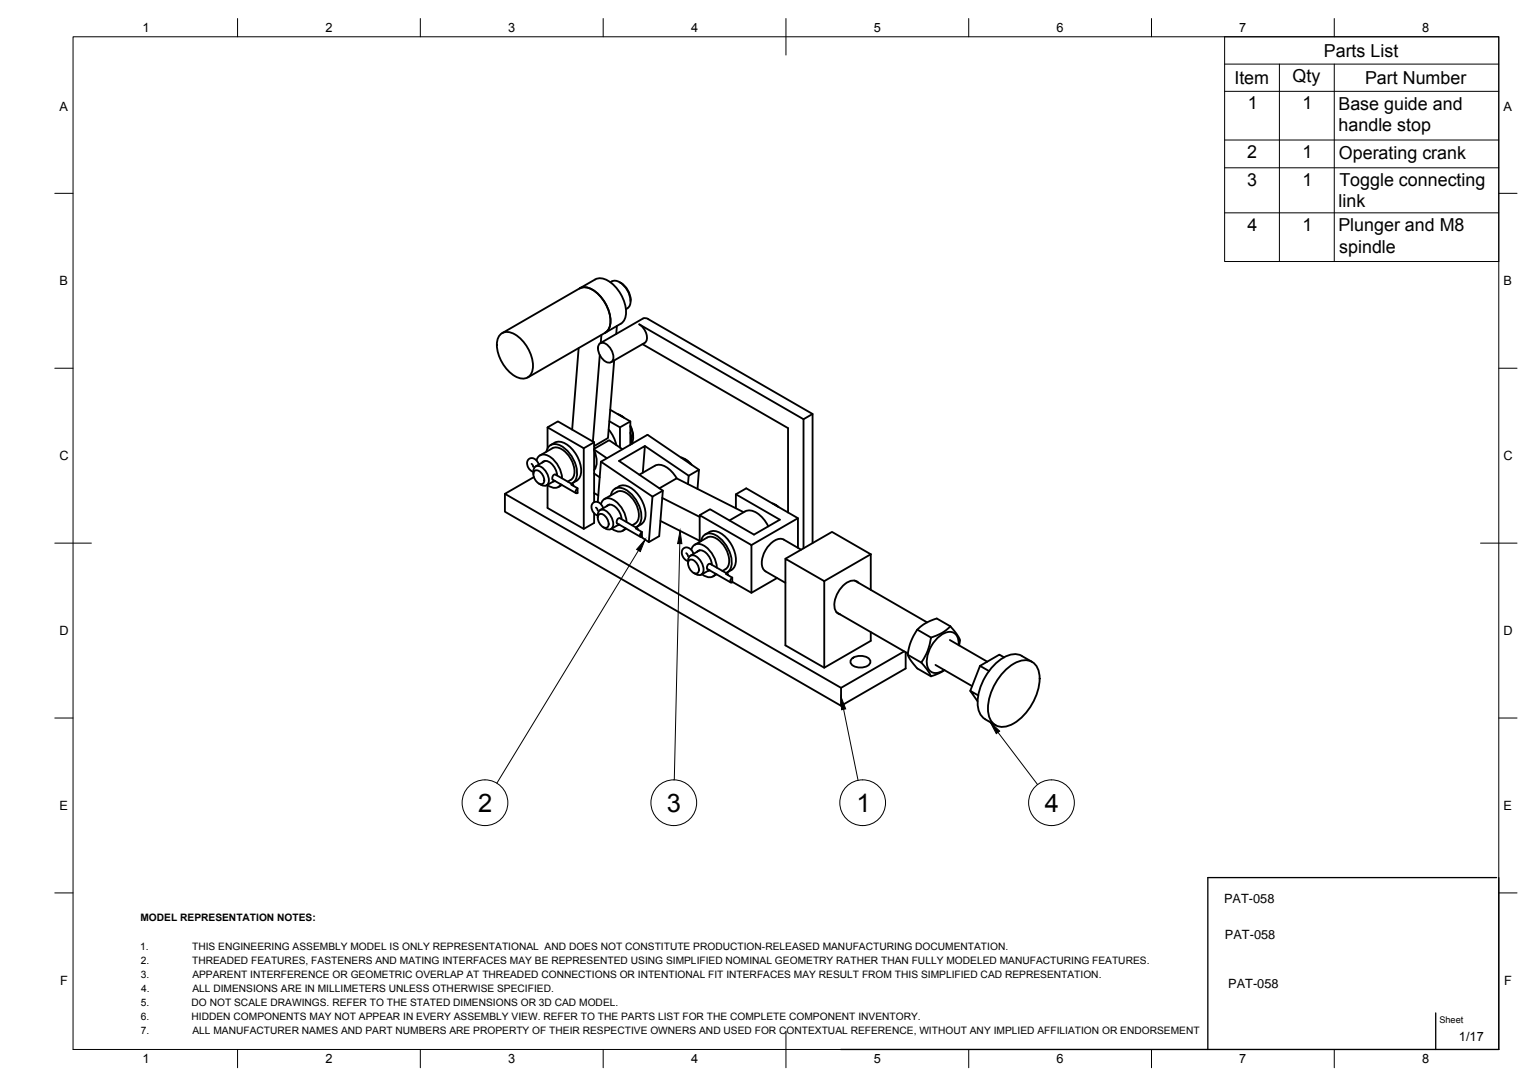
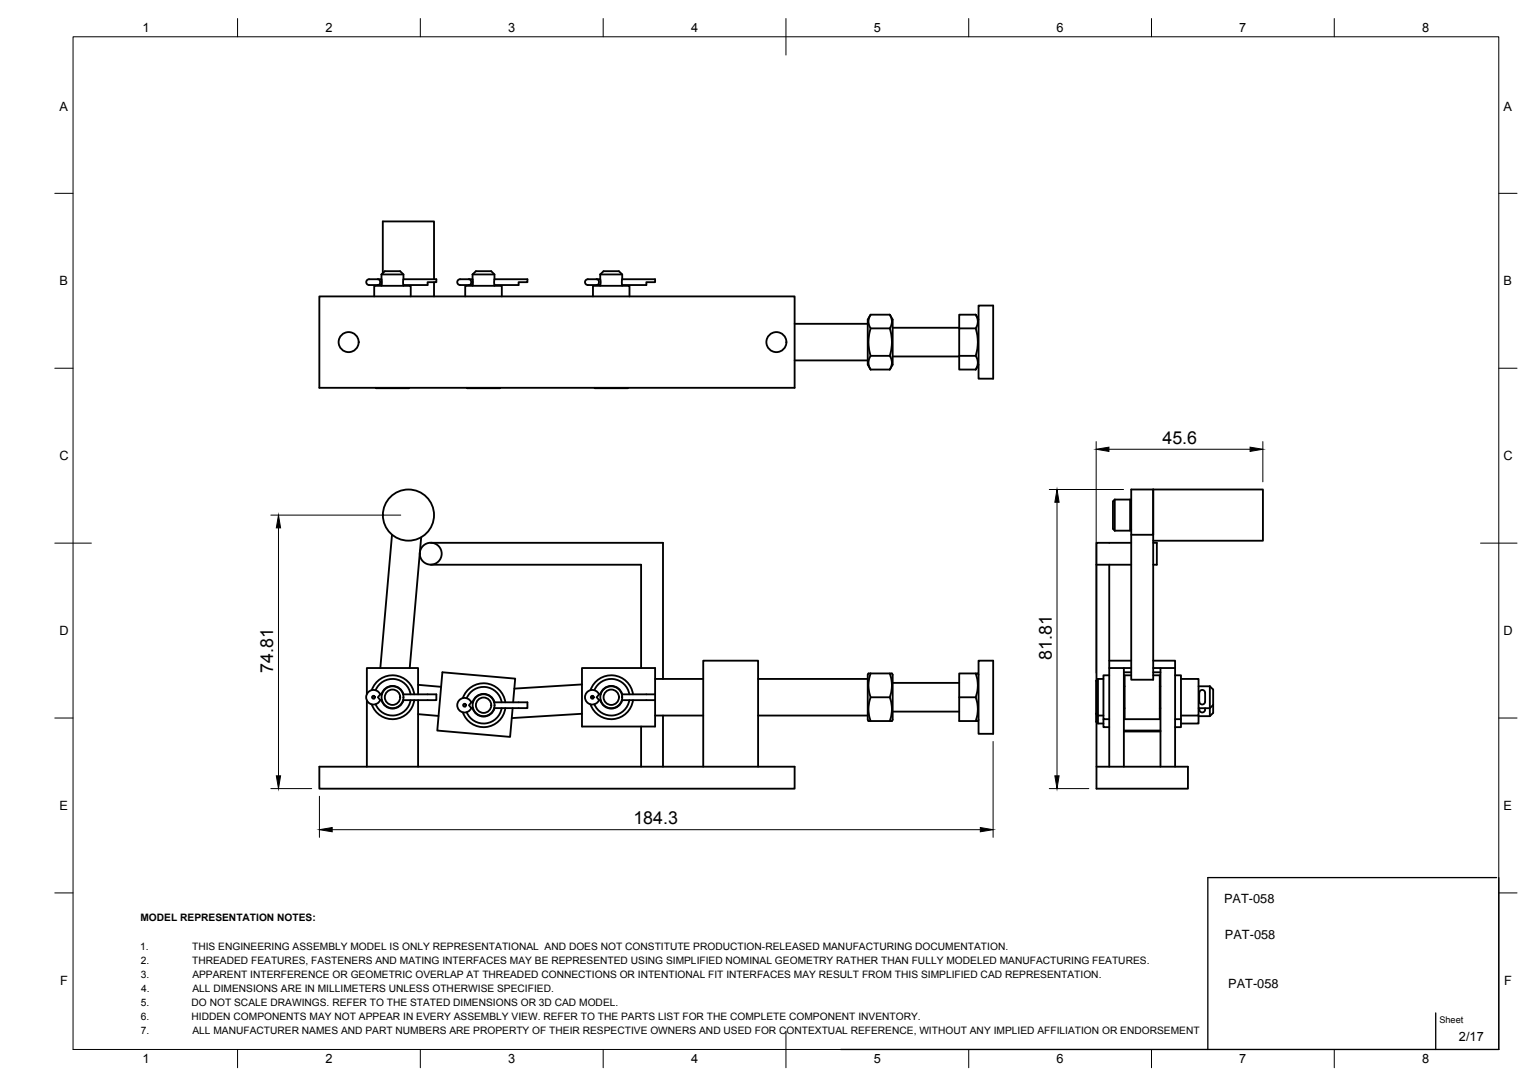
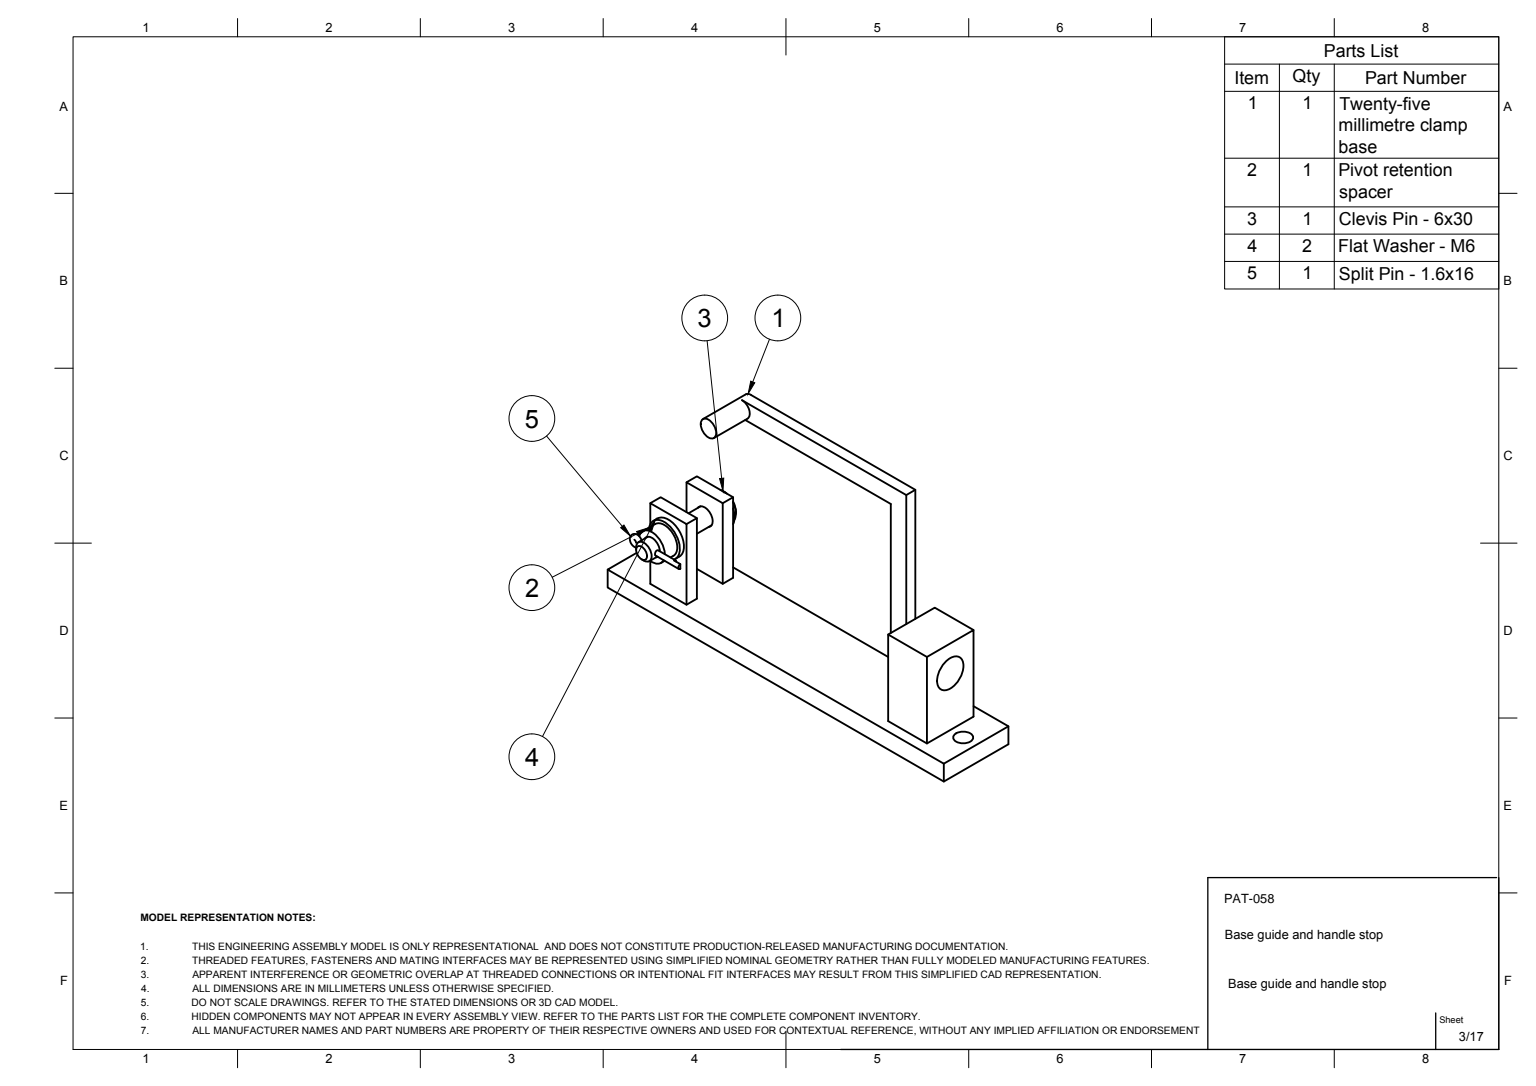
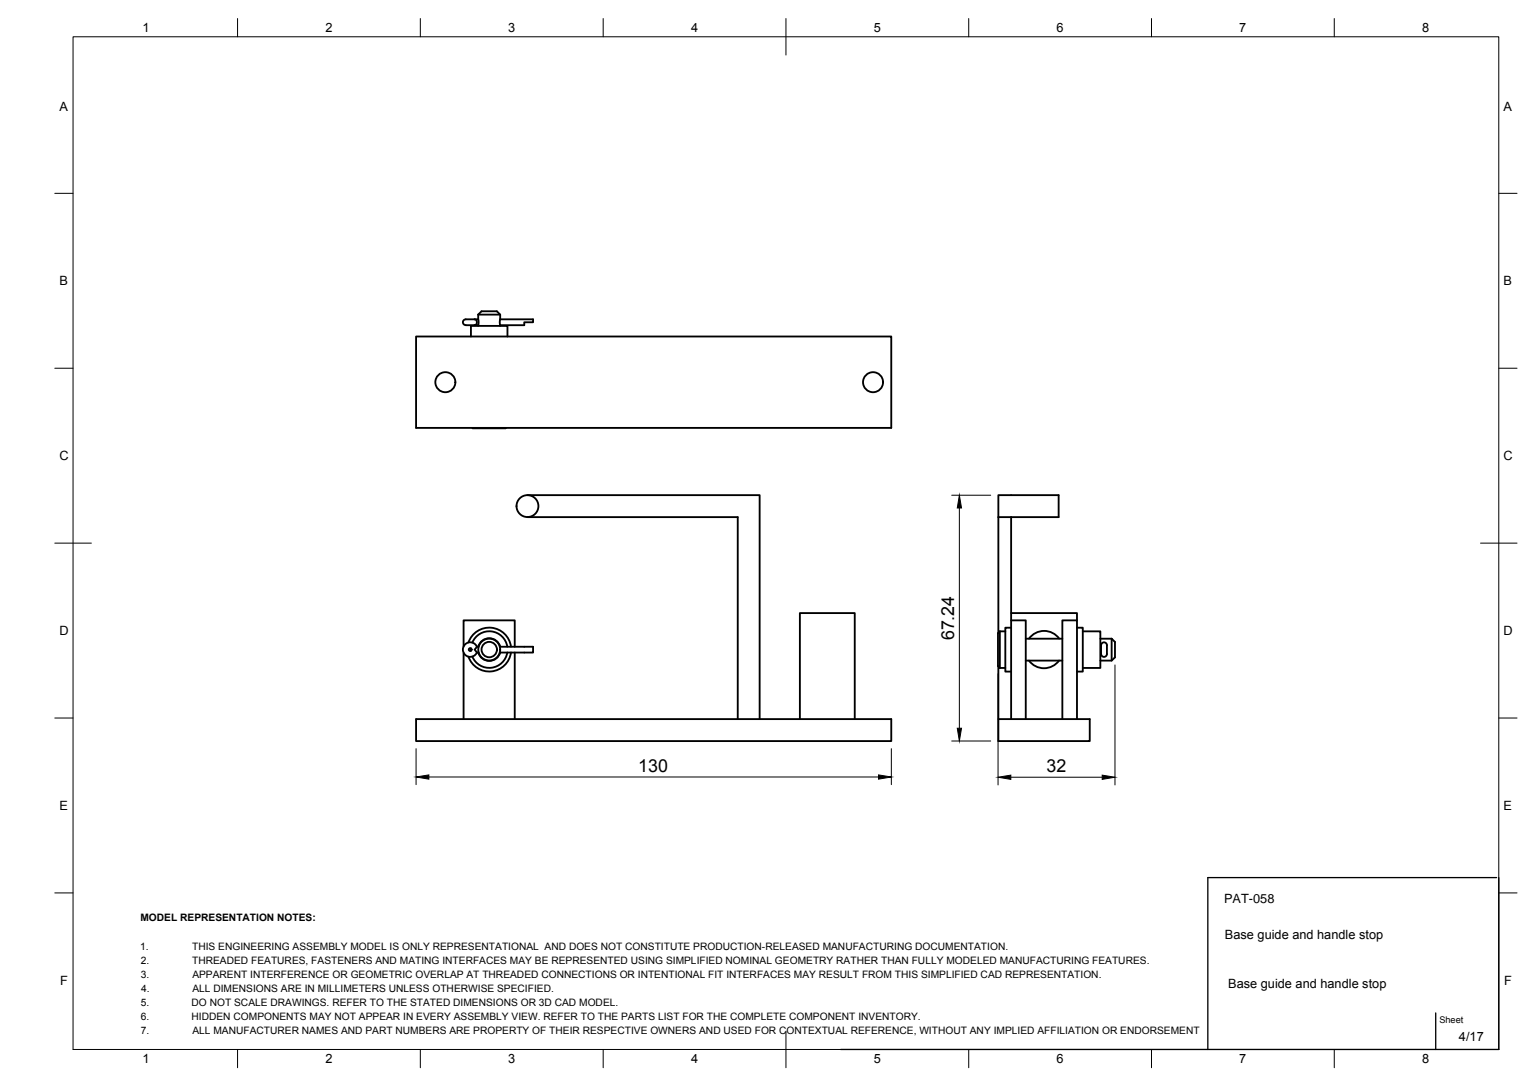
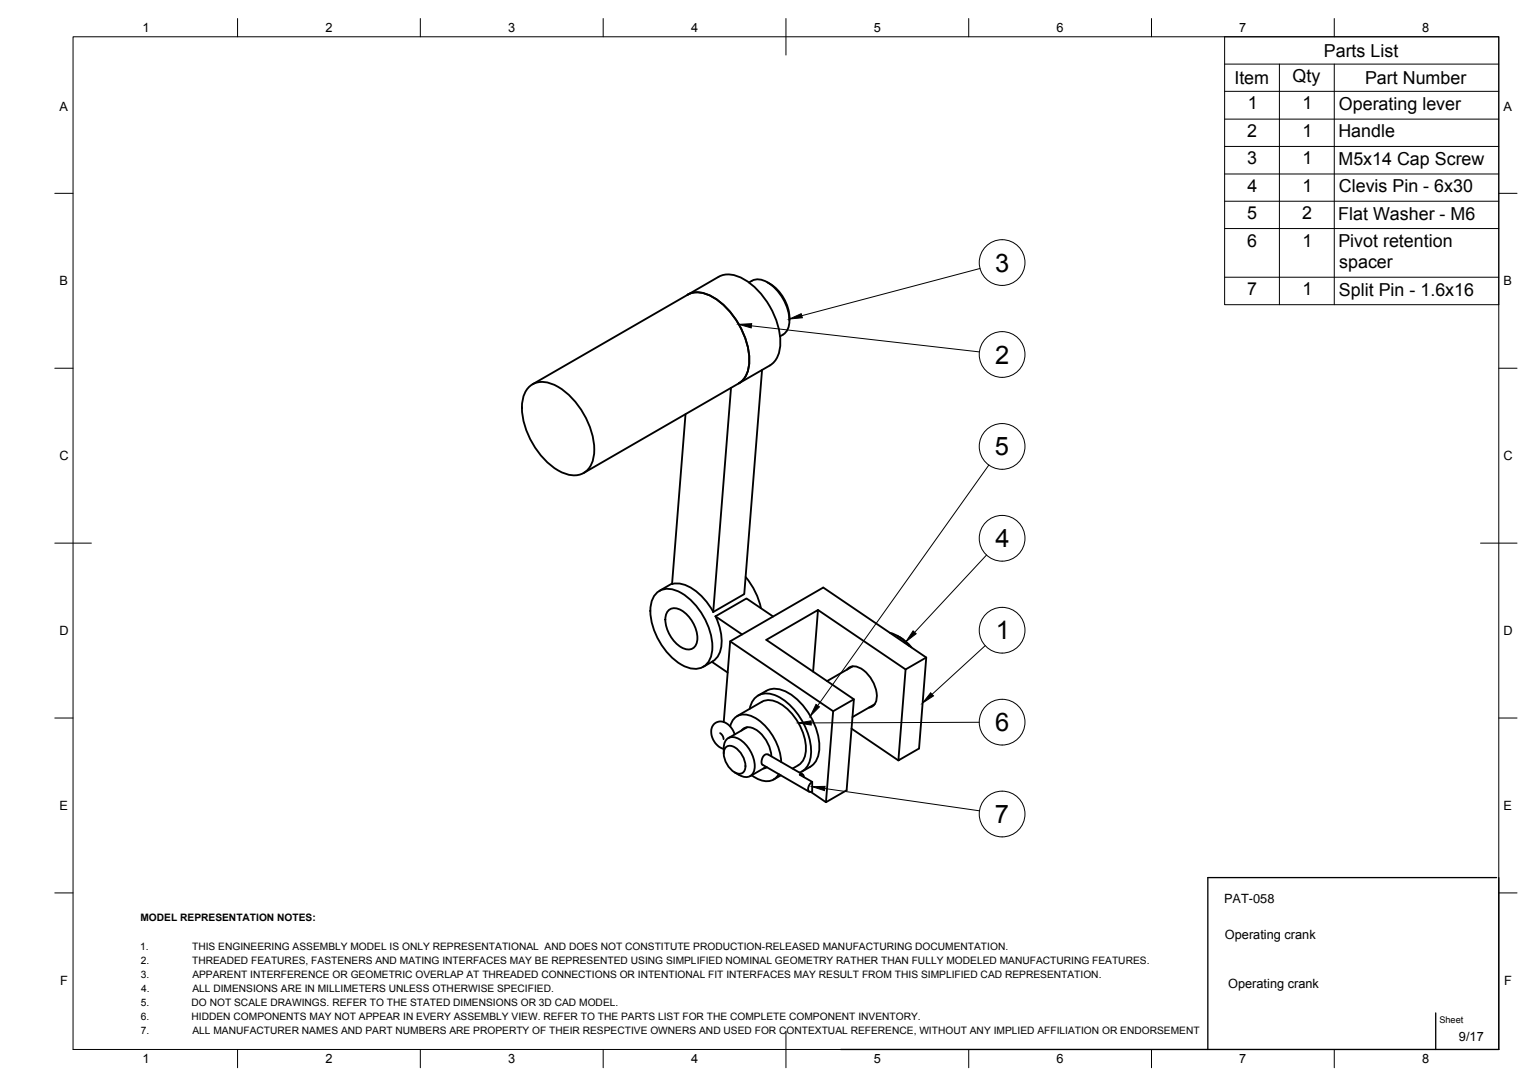
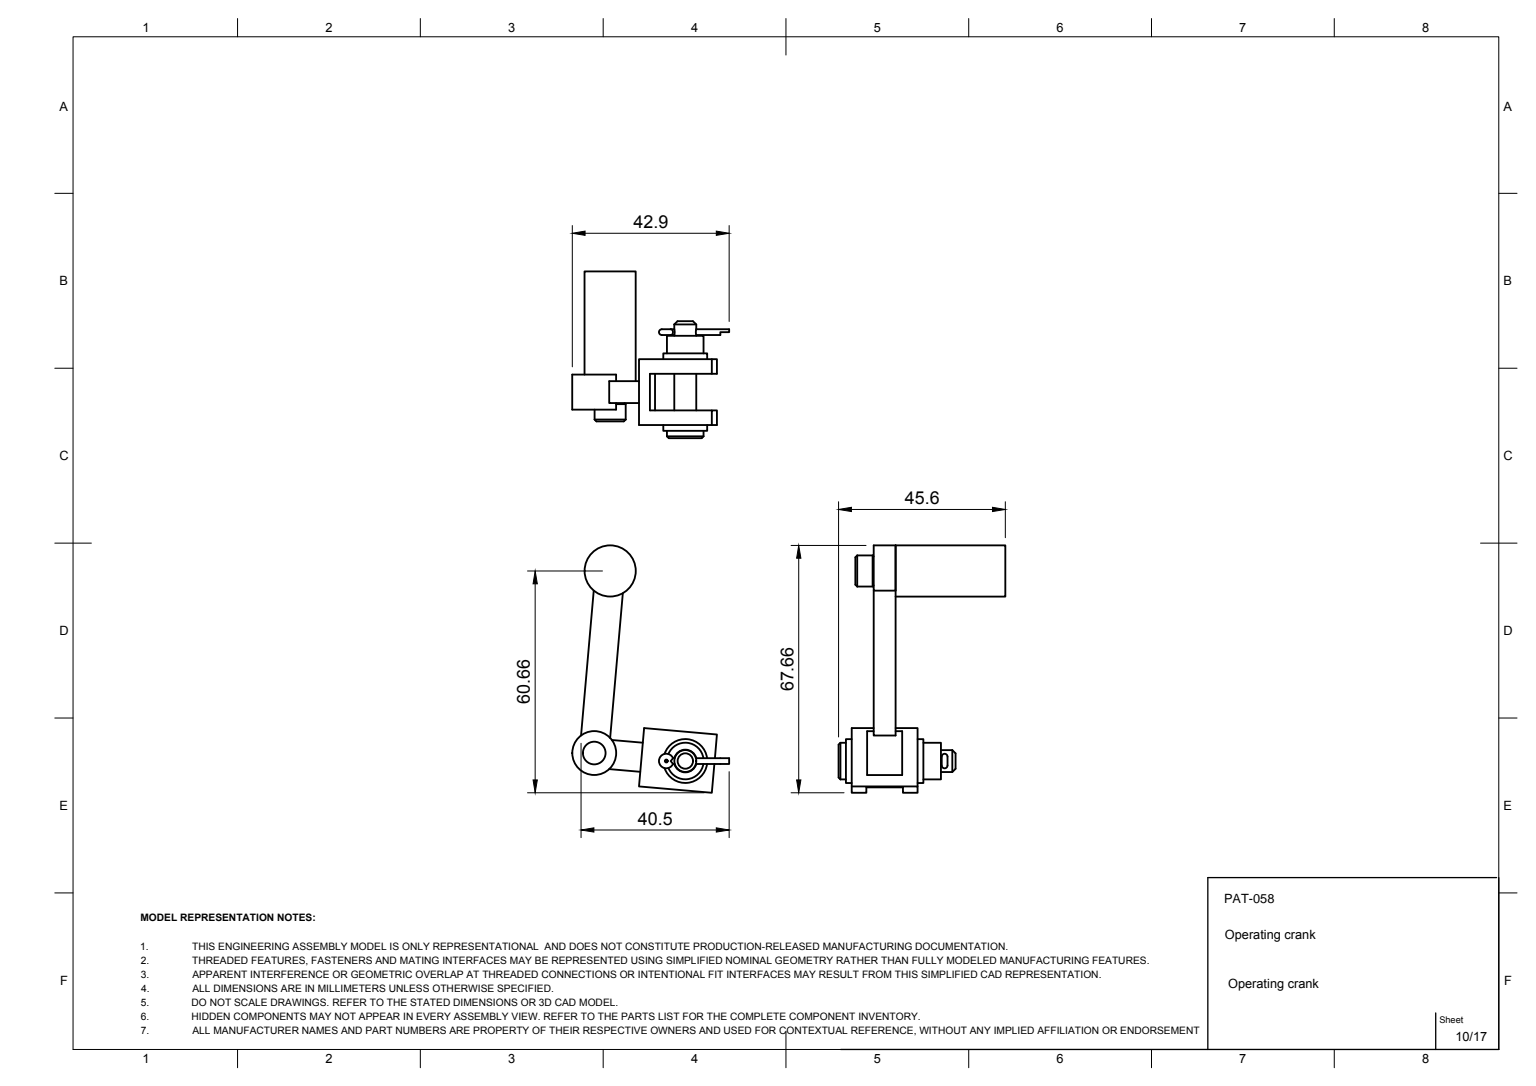
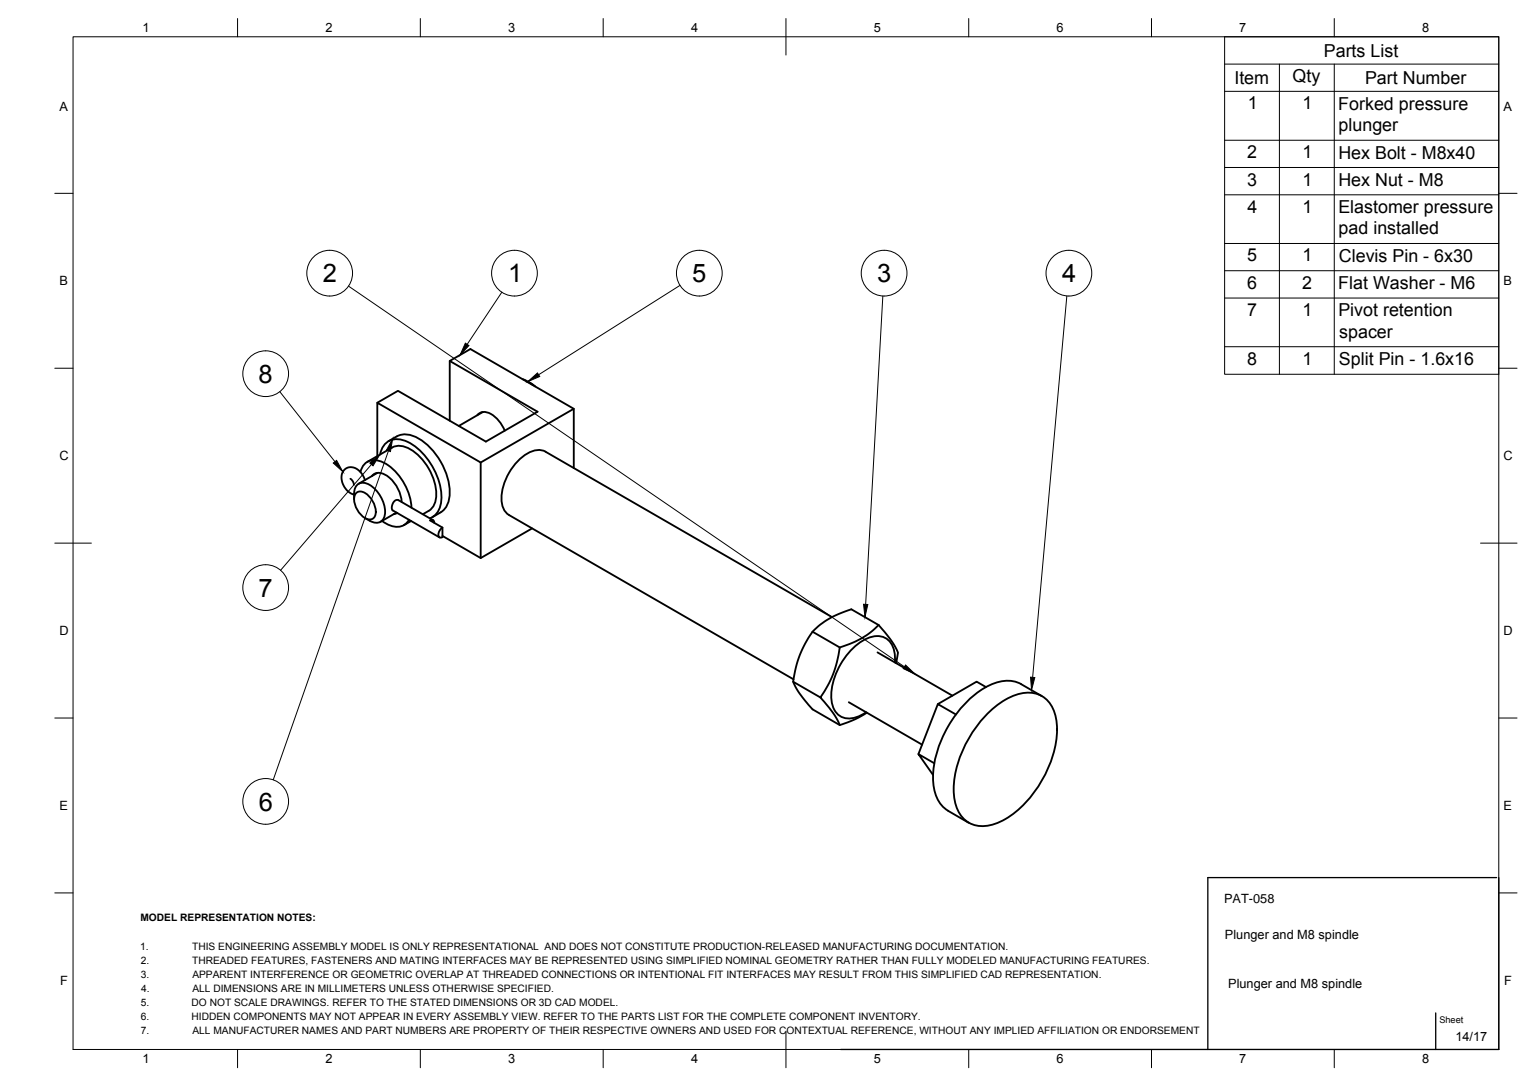
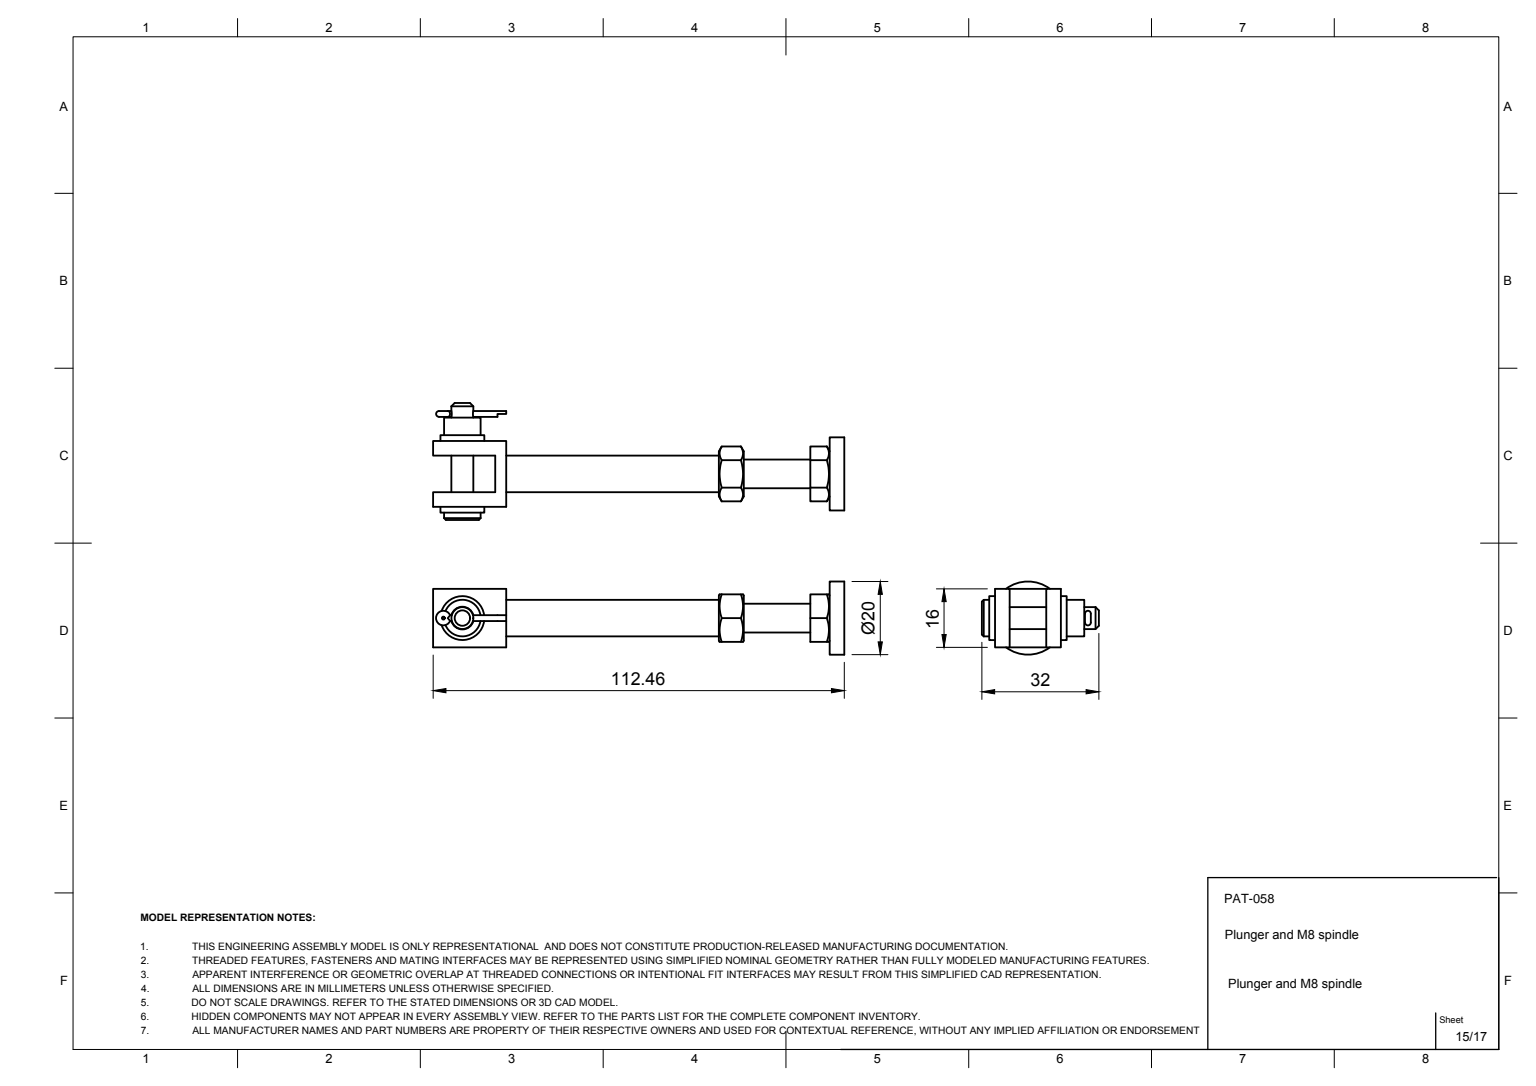
ISO-10303-21;
HEADER;
/* Generated by software containing ST-Developer
 * from STEP Tools, Inc. (www.steptools.com) 
 */

FILE_DESCRIPTION(
/* description */ ('Horizontal push-pull toggle clamp'),
/* implementation_level */ '2;1');

FILE_NAME(
/* name */ 'PAT-058',
/* time_stamp */ '2026-10-27T21:21:09-07:00',
/* author */ (''),
/* organization */ (''),
/* preprocessor_version */ 'ST-DEVELOPER v20.2',
/* originating_system */ 'Autodesk Translation Framework v15.17.0.0',
/* authorisation */ '');

FILE_SCHEMA (('AUTOMOTIVE_DESIGN { 1 0 10303 214 3 1 1 }'));
ENDSEC;

DATA;
#10=MECHANICAL_DESIGN_GEOMETRIC_PRESENTATION_REPRESENTATION('',(#185,#186,
#187,#188,#189,#190,#191,#192,#193,#194,#195,#196,#197),#4791);
#11=TOROIDAL_SURFACE('',#3033,0.12,0.08);
#12=B_SPLINE_CURVE_WITH_KNOTS('',3,(#4522,#4523,#4524,#4525,#4526,#4527,
#4528,#4529,#4530,#4531),.UNSPECIFIED.,.F.,.F.,(4,2,2,2,4),(0.,0.0302963256060356,
0.0605926512120712,0.090883446720838,0.121174242229605),.UNSPECIFIED.);
#13=B_SPLINE_CURVE_WITH_KNOTS('',3,(#4534,#4535,#4536,#4537,#4538,#4539,
#4540,#4541,#4542,#4543,#4544,#4545,#4546,#4547,#4548,#4549,#4550,#4551,
#4552,#4553,#4554,#4555,#4556,#4557,#4558,#4559,#4560,#4561,#4562,#4563,
#4564,#4565,#4566,#4567),.UNSPECIFIED.,.T.,.F.,(4,2,2,2,2,2,2,2,2,2,2,2,
2,2,2,2,4),(0.,0.0302963256060358,0.0605926512120716,0.0908834467208383,
0.121174242229605,0.151465037738372,0.181755833247138,0.212052158853174,
0.24234848445921,0.272644810065246,0.302941135671282,0.333231931180048,
0.363522726688815,0.393813522197582,0.424104317706349,0.454400643312384,
0.48469696891842),.UNSPECIFIED.);
#14=B_SPLINE_CURVE_WITH_KNOTS('',3,(#4569,#4570,#4571,#4572,#4573,#4574,
#4575,#4576,#4577,#4578),.UNSPECIFIED.,.F.,.F.,(4,2,2,2,4),(0.363522726688815,
0.393813522197581,0.424104317706348,0.454400643312384,0.48469696891842),
 .UNSPECIFIED.);
#15=B_SPLINE_CURVE_WITH_KNOTS('',3,(#4579,#4580,#4581,#4582,#4583,#4584,
#4585,#4586,#4587,#4588,#4589,#4590,#4591,#4592,#4593,#4594,#4595,#4596),
 .UNSPECIFIED.,.F.,.F.,(4,2,2,2,2,2,2,2,4),(0.121174242229605,0.151465037738371,
0.181755833247138,0.212052158853174,0.24234848445921,0.272644810065246,
0.302941135671281,0.333231931180048,0.363522726688815),.UNSPECIFIED.);
#16=B_SPLINE_CURVE_WITH_KNOTS('',3,(#4658,#4659,#4660,#4661,#4662,#4663,
#4664,#4665,#4666,#4667,#4668,#4669,#4670,#4671,#4672,#4673,#4674,#4675,
#4676,#4677,#4678,#4679,#4680,#4681,#4682,#4683),.UNSPECIFIED.,.F.,.F.,
(4,2,2,2,2,2,2,2,2,2,2,2,4),(-0.00054581412719389,0.,0.0281583564005144,
0.0618496465371181,0.0905865724114538,0.120694112793616,0.144966158459363,
0.16923820412511,0.199345744507272,0.228082670381608,0.261773960518212,
0.289932316918681,0.290478131045882),.UNSPECIFIED.);
#17=B_SPLINE_CURVE_WITH_KNOTS('',3,(#4684,#4685,#4686,#4687,#4688,#4689,
#4690,#4691,#4692,#4693,#4694,#4695,#4696,#4697,#4698,#4699,#4700,#4701,
#4702,#4703,#4704,#4705,#4706,#4707,#4708,#4709),.UNSPECIFIED.,.F.,.F.,
(4,2,2,2,2,2,2,2,2,2,2,2,4),(-0.000545814127196571,0.,0.0281583564006391,
0.0618496465374156,0.0905865724118984,0.120694112794215,0.144966158460086,
0.169238204125958,0.199345744508275,0.228082670382758,0.261773960519534,
0.289932316920171,0.29047813104737),.UNSPECIFIED.);
#18=(
BOUNDED_CURVE()
B_SPLINE_CURVE(2,(#4384,#4385,#4386),.UNSPECIFIED.,.F.,.F.)
B_SPLINE_CURVE_WITH_KNOTS((3,3),(0.14973948338295,0.97160236658079),
 .UNSPECIFIED.)
CURVE()
GEOMETRIC_REPRESENTATION_ITEM()
RATIONAL_B_SPLINE_CURVE((1.07140024848292,1.23714644374248,1.07140024848292))
REPRESENTATION_ITEM('')
);
#19=(
BOUNDED_CURVE()
B_SPLINE_CURVE(2,(#4388,#4389,#4390),.UNSPECIFIED.,.F.,.F.)
B_SPLINE_CURVE_WITH_KNOTS((3,3),(0.14973948338295,0.97160236658079),
 .UNSPECIFIED.)
CURVE()
GEOMETRIC_REPRESENTATION_ITEM()
RATIONAL_B_SPLINE_CURVE((1.07140024848292,1.23714644374248,1.07140024848292))
REPRESENTATION_ITEM('')
);
#20=(
BOUNDED_CURVE()
B_SPLINE_CURVE(2,(#4392,#4393,#4394),.UNSPECIFIED.,.F.,.F.)
B_SPLINE_CURVE_WITH_KNOTS((3,3),(0.14973948338295,0.97160236658079),
 .UNSPECIFIED.)
CURVE()
GEOMETRIC_REPRESENTATION_ITEM()
RATIONAL_B_SPLINE_CURVE((1.07140024848292,1.23714644374248,1.07140024848292))
REPRESENTATION_ITEM('')
);
#21=(
BOUNDED_CURVE()
B_SPLINE_CURVE(2,(#4396,#4397,#4398),.UNSPECIFIED.,.F.,.F.)
B_SPLINE_CURVE_WITH_KNOTS((3,3),(0.149739483382949,0.971602366580789),
 .UNSPECIFIED.)
CURVE()
GEOMETRIC_REPRESENTATION_ITEM()
RATIONAL_B_SPLINE_CURVE((1.07140024848292,1.23714644374248,1.07140024848292))
REPRESENTATION_ITEM('')
);
#22=(
BOUNDED_CURVE()
B_SPLINE_CURVE(2,(#4400,#4401,#4402),.UNSPECIFIED.,.F.,.F.)
B_SPLINE_CURVE_WITH_KNOTS((3,3),(0.14973948338295,0.971602366580789),
 .UNSPECIFIED.)
CURVE()
GEOMETRIC_REPRESENTATION_ITEM()
RATIONAL_B_SPLINE_CURVE((1.07140024848292,1.23714644374248,1.07140024848292))
REPRESENTATION_ITEM('')
);
#23=(
BOUNDED_CURVE()
B_SPLINE_CURVE(2,(#4403,#4404,#4405),.UNSPECIFIED.,.F.,.F.)
B_SPLINE_CURVE_WITH_KNOTS((3,3),(0.14973948338295,0.97160236658079),
 .UNSPECIFIED.)
CURVE()
GEOMETRIC_REPRESENTATION_ITEM()
RATIONAL_B_SPLINE_CURVE((1.07140024848292,1.23714644374248,1.07140024848292))
REPRESENTATION_ITEM('')
);
#24=(
BOUNDED_CURVE()
B_SPLINE_CURVE(2,(#4436,#4437,#4438),.UNSPECIFIED.,.F.,.F.)
B_SPLINE_CURVE_WITH_KNOTS((3,3),(0.14973948338295,0.97160236658079),
 .UNSPECIFIED.)
CURVE()
GEOMETRIC_REPRESENTATION_ITEM()
RATIONAL_B_SPLINE_CURVE((1.07140024848292,1.23714644374248,1.07140024848292))
REPRESENTATION_ITEM('')
);
#25=(
BOUNDED_CURVE()
B_SPLINE_CURVE(2,(#4440,#4441,#4442),.UNSPECIFIED.,.F.,.F.)
B_SPLINE_CURVE_WITH_KNOTS((3,3),(0.14973948338295,0.971602366580789),
 .UNSPECIFIED.)
CURVE()
GEOMETRIC_REPRESENTATION_ITEM()
RATIONAL_B_SPLINE_CURVE((1.07140024848292,1.23714644374248,1.07140024848292))
REPRESENTATION_ITEM('')
);
#26=(
BOUNDED_CURVE()
B_SPLINE_CURVE(2,(#4447,#4448,#4449),.UNSPECIFIED.,.F.,.F.)
B_SPLINE_CURVE_WITH_KNOTS((3,3),(0.14973948338295,0.97160236658079),
 .UNSPECIFIED.)
CURVE()
GEOMETRIC_REPRESENTATION_ITEM()
RATIONAL_B_SPLINE_CURVE((1.07140024848292,1.23714644374248,1.07140024848292))
REPRESENTATION_ITEM('')
);
#27=(
BOUNDED_CURVE()
B_SPLINE_CURVE(2,(#4451,#4452,#4453),.UNSPECIFIED.,.F.,.F.)
B_SPLINE_CURVE_WITH_KNOTS((3,3),(0.14973948338295,0.97160236658079),
 .UNSPECIFIED.)
CURVE()
GEOMETRIC_REPRESENTATION_ITEM()
RATIONAL_B_SPLINE_CURVE((1.07140024848292,1.23714644374248,1.07140024848292))
REPRESENTATION_ITEM('')
);
#28=(
BOUNDED_CURVE()
B_SPLINE_CURVE(2,(#4455,#4456,#4457),.UNSPECIFIED.,.F.,.F.)
B_SPLINE_CURVE_WITH_KNOTS((3,3),(0.14973948338295,0.971602366580789),
 .UNSPECIFIED.)
CURVE()
GEOMETRIC_REPRESENTATION_ITEM()
RATIONAL_B_SPLINE_CURVE((1.07140024848292,1.23714644374248,1.07140024848292))
REPRESENTATION_ITEM('')
);
#29=(
BOUNDED_CURVE()
B_SPLINE_CURVE(2,(#4458,#4459,#4460),.UNSPECIFIED.,.F.,.F.)
B_SPLINE_CURVE_WITH_KNOTS((3,3),(0.14973948338295,0.97160236658079),
 .UNSPECIFIED.)
CURVE()
GEOMETRIC_REPRESENTATION_ITEM()
RATIONAL_B_SPLINE_CURVE((1.07140024848292,1.23714644374248,1.07140024848292))
REPRESENTATION_ITEM('')
);
#30=(
BOUNDED_CURVE()
B_SPLINE_CURVE(2,(#4467,#4468,#4469),.UNSPECIFIED.,.F.,.F.)
B_SPLINE_CURVE_WITH_KNOTS((3,3),(0.14973948338295,0.97160236658079),
 .UNSPECIFIED.)
CURVE()
GEOMETRIC_REPRESENTATION_ITEM()
RATIONAL_B_SPLINE_CURVE((1.07140024848292,1.23714644374248,1.07140024848292))
REPRESENTATION_ITEM('')
);
#31=(
BOUNDED_CURVE()
B_SPLINE_CURVE(2,(#4471,#4472,#4473),.UNSPECIFIED.,.F.,.F.)
B_SPLINE_CURVE_WITH_KNOTS((3,3),(0.14973948338295,0.97160236658079),
 .UNSPECIFIED.)
CURVE()
GEOMETRIC_REPRESENTATION_ITEM()
RATIONAL_B_SPLINE_CURVE((1.07140024848292,1.23714644374248,1.07140024848292))
REPRESENTATION_ITEM('')
);
#32=(
BOUNDED_CURVE()
B_SPLINE_CURVE(2,(#4475,#4476,#4477),.UNSPECIFIED.,.F.,.F.)
B_SPLINE_CURVE_WITH_KNOTS((3,3),(0.14973948338295,0.971602366580789),
 .UNSPECIFIED.)
CURVE()
GEOMETRIC_REPRESENTATION_ITEM()
RATIONAL_B_SPLINE_CURVE((1.07140024848292,1.23714644374248,1.07140024848292))
REPRESENTATION_ITEM('')
);
#33=(
BOUNDED_CURVE()
B_SPLINE_CURVE(2,(#4479,#4480,#4481),.UNSPECIFIED.,.F.,.F.)
B_SPLINE_CURVE_WITH_KNOTS((3,3),(0.14973948338295,0.97160236658079),
 .UNSPECIFIED.)
CURVE()
GEOMETRIC_REPRESENTATION_ITEM()
RATIONAL_B_SPLINE_CURVE((1.07140024848292,1.23714644374248,1.07140024848292))
REPRESENTATION_ITEM('')
);
#34=(
BOUNDED_CURVE()
B_SPLINE_CURVE(2,(#4483,#4484,#4485),.UNSPECIFIED.,.F.,.F.)
B_SPLINE_CURVE_WITH_KNOTS((3,3),(0.14973948338295,0.97160236658079),
 .UNSPECIFIED.)
CURVE()
GEOMETRIC_REPRESENTATION_ITEM()
RATIONAL_B_SPLINE_CURVE((1.07140024848292,1.23714644374248,1.07140024848292))
REPRESENTATION_ITEM('')
);
#35=(
BOUNDED_CURVE()
B_SPLINE_CURVE(2,(#4486,#4487,#4488),.UNSPECIFIED.,.F.,.F.)
B_SPLINE_CURVE_WITH_KNOTS((3,3),(0.14973948338295,0.971602366580789),
 .UNSPECIFIED.)
CURVE()
GEOMETRIC_REPRESENTATION_ITEM()
RATIONAL_B_SPLINE_CURVE((1.07140024848292,1.23714644374248,1.07140024848292))
REPRESENTATION_ITEM('')
);
#36=ITEM_DEFINED_TRANSFORMATION($,$,#2916,#2933);
#37=ITEM_DEFINED_TRANSFORMATION($,$,#2789,#3043);
#38=ITEM_DEFINED_TRANSFORMATION($,$,#3023,#3044);
#39=ITEM_DEFINED_TRANSFORMATION($,$,#2999,#3045);
#40=ITEM_DEFINED_TRANSFORMATION($,$,#3014,#3046);
#41=ITEM_DEFINED_TRANSFORMATION($,$,#3014,#3047);
#42=ITEM_DEFINED_TRANSFORMATION($,$,#3032,#3048);
#43=ITEM_DEFINED_TRANSFORMATION($,$,#2838,#3049);
#44=ITEM_DEFINED_TRANSFORMATION($,$,#2881,#3050);
#45=ITEM_DEFINED_TRANSFORMATION($,$,#2891,#3051);
#46=ITEM_DEFINED_TRANSFORMATION($,$,#2999,#3052);
#47=ITEM_DEFINED_TRANSFORMATION($,$,#3014,#3053);
#48=ITEM_DEFINED_TRANSFORMATION($,$,#3014,#3054);
#49=ITEM_DEFINED_TRANSFORMATION($,$,#3023,#3055);
#50=ITEM_DEFINED_TRANSFORMATION($,$,#3032,#3056);
#51=ITEM_DEFINED_TRANSFORMATION($,$,#2935,#3057);
#52=ITEM_DEFINED_TRANSFORMATION($,$,#2960,#3058);
#53=ITEM_DEFINED_TRANSFORMATION($,$,#2977,#3059);
#54=ITEM_DEFINED_TRANSFORMATION($,$,#2993,#3060);
#55=ITEM_DEFINED_TRANSFORMATION($,$,#2999,#3061);
#56=ITEM_DEFINED_TRANSFORMATION($,$,#3014,#3062);
#57=ITEM_DEFINED_TRANSFORMATION($,$,#3014,#3063);
#58=ITEM_DEFINED_TRANSFORMATION($,$,#3023,#3064);
#59=ITEM_DEFINED_TRANSFORMATION($,$,#3032,#3065);
#60=ITEM_DEFINED_TRANSFORMATION($,$,#2788,#3066);
#61=ITEM_DEFINED_TRANSFORMATION($,$,#2837,#3067);
#62=ITEM_DEFINED_TRANSFORMATION($,$,#2915,#3068);
#63=ITEM_DEFINED_TRANSFORMATION($,$,#2934,#3069);
#64=(
REPRESENTATION_RELATIONSHIP($,$,#4868,#4867)
REPRESENTATION_RELATIONSHIP_WITH_TRANSFORMATION(#36)
SHAPE_REPRESENTATION_RELATIONSHIP()
);
#65=(
REPRESENTATION_RELATIONSHIP($,$,#4862,#4861)
REPRESENTATION_RELATIONSHIP_WITH_TRANSFORMATION(#37)
SHAPE_REPRESENTATION_RELATIONSHIP()
);
#66=(
REPRESENTATION_RELATIONSHIP($,$,#4876,#4861)
REPRESENTATION_RELATIONSHIP_WITH_TRANSFORMATION(#38)
SHAPE_REPRESENTATION_RELATIONSHIP()
);
#67=(
REPRESENTATION_RELATIONSHIP($,$,#4874,#4861)
REPRESENTATION_RELATIONSHIP_WITH_TRANSFORMATION(#39)
SHAPE_REPRESENTATION_RELATIONSHIP()
);
#68=(
REPRESENTATION_RELATIONSHIP($,$,#4875,#4861)
REPRESENTATION_RELATIONSHIP_WITH_TRANSFORMATION(#40)
SHAPE_REPRESENTATION_RELATIONSHIP()
);
#69=(
REPRESENTATION_RELATIONSHIP($,$,#4875,#4861)
REPRESENTATION_RELATIONSHIP_WITH_TRANSFORMATION(#41)
SHAPE_REPRESENTATION_RELATIONSHIP()
);
#70=(
REPRESENTATION_RELATIONSHIP($,$,#4877,#4861)
REPRESENTATION_RELATIONSHIP_WITH_TRANSFORMATION(#42)
SHAPE_REPRESENTATION_RELATIONSHIP()
);
#71=(
REPRESENTATION_RELATIONSHIP($,$,#4864,#4863)
REPRESENTATION_RELATIONSHIP_WITH_TRANSFORMATION(#43)
SHAPE_REPRESENTATION_RELATIONSHIP()
);
#72=(
REPRESENTATION_RELATIONSHIP($,$,#4865,#4863)
REPRESENTATION_RELATIONSHIP_WITH_TRANSFORMATION(#44)
SHAPE_REPRESENTATION_RELATIONSHIP()
);
#73=(
REPRESENTATION_RELATIONSHIP($,$,#4866,#4863)
REPRESENTATION_RELATIONSHIP_WITH_TRANSFORMATION(#45)
SHAPE_REPRESENTATION_RELATIONSHIP()
);
#74=(
REPRESENTATION_RELATIONSHIP($,$,#4874,#4863)
REPRESENTATION_RELATIONSHIP_WITH_TRANSFORMATION(#46)
SHAPE_REPRESENTATION_RELATIONSHIP()
);
#75=(
REPRESENTATION_RELATIONSHIP($,$,#4875,#4863)
REPRESENTATION_RELATIONSHIP_WITH_TRANSFORMATION(#47)
SHAPE_REPRESENTATION_RELATIONSHIP()
);
#76=(
REPRESENTATION_RELATIONSHIP($,$,#4875,#4863)
REPRESENTATION_RELATIONSHIP_WITH_TRANSFORMATION(#48)
SHAPE_REPRESENTATION_RELATIONSHIP()
);
#77=(
REPRESENTATION_RELATIONSHIP($,$,#4876,#4863)
REPRESENTATION_RELATIONSHIP_WITH_TRANSFORMATION(#49)
SHAPE_REPRESENTATION_RELATIONSHIP()
);
#78=(
REPRESENTATION_RELATIONSHIP($,$,#4877,#4863)
REPRESENTATION_RELATIONSHIP_WITH_TRANSFORMATION(#50)
SHAPE_REPRESENTATION_RELATIONSHIP()
);
#79=(
REPRESENTATION_RELATIONSHIP($,$,#4870,#4869)
REPRESENTATION_RELATIONSHIP_WITH_TRANSFORMATION(#51)
SHAPE_REPRESENTATION_RELATIONSHIP()
);
#80=(
REPRESENTATION_RELATIONSHIP($,$,#4871,#4869)
REPRESENTATION_RELATIONSHIP_WITH_TRANSFORMATION(#52)
SHAPE_REPRESENTATION_RELATIONSHIP()
);
#81=(
REPRESENTATION_RELATIONSHIP($,$,#4872,#4869)
REPRESENTATION_RELATIONSHIP_WITH_TRANSFORMATION(#53)
SHAPE_REPRESENTATION_RELATIONSHIP()
);
#82=(
REPRESENTATION_RELATIONSHIP($,$,#4873,#4869)
REPRESENTATION_RELATIONSHIP_WITH_TRANSFORMATION(#54)
SHAPE_REPRESENTATION_RELATIONSHIP()
);
#83=(
REPRESENTATION_RELATIONSHIP($,$,#4874,#4869)
REPRESENTATION_RELATIONSHIP_WITH_TRANSFORMATION(#55)
SHAPE_REPRESENTATION_RELATIONSHIP()
);
#84=(
REPRESENTATION_RELATIONSHIP($,$,#4875,#4869)
REPRESENTATION_RELATIONSHIP_WITH_TRANSFORMATION(#56)
SHAPE_REPRESENTATION_RELATIONSHIP()
);
#85=(
REPRESENTATION_RELATIONSHIP($,$,#4875,#4869)
REPRESENTATION_RELATIONSHIP_WITH_TRANSFORMATION(#57)
SHAPE_REPRESENTATION_RELATIONSHIP()
);
#86=(
REPRESENTATION_RELATIONSHIP($,$,#4876,#4869)
REPRESENTATION_RELATIONSHIP_WITH_TRANSFORMATION(#58)
SHAPE_REPRESENTATION_RELATIONSHIP()
);
#87=(
REPRESENTATION_RELATIONSHIP($,$,#4877,#4869)
REPRESENTATION_RELATIONSHIP_WITH_TRANSFORMATION(#59)
SHAPE_REPRESENTATION_RELATIONSHIP()
);
#88=(
REPRESENTATION_RELATIONSHIP($,$,#4861,#4860)
REPRESENTATION_RELATIONSHIP_WITH_TRANSFORMATION(#60)
SHAPE_REPRESENTATION_RELATIONSHIP()
);
#89=(
REPRESENTATION_RELATIONSHIP($,$,#4863,#4860)
REPRESENTATION_RELATIONSHIP_WITH_TRANSFORMATION(#61)
SHAPE_REPRESENTATION_RELATIONSHIP()
);
#90=(
REPRESENTATION_RELATIONSHIP($,$,#4867,#4860)
REPRESENTATION_RELATIONSHIP_WITH_TRANSFORMATION(#62)
SHAPE_REPRESENTATION_RELATIONSHIP()
);
#91=(
REPRESENTATION_RELATIONSHIP($,$,#4869,#4860)
REPRESENTATION_RELATIONSHIP_WITH_TRANSFORMATION(#63)
SHAPE_REPRESENTATION_RELATIONSHIP()
);
#92=CONTEXT_DEPENDENT_SHAPE_REPRESENTATION(#64,#4823);
#93=CONTEXT_DEPENDENT_SHAPE_REPRESENTATION(#65,#4833);
#94=CONTEXT_DEPENDENT_SHAPE_REPRESENTATION(#66,#4834);
#95=CONTEXT_DEPENDENT_SHAPE_REPRESENTATION(#67,#4835);
#96=CONTEXT_DEPENDENT_SHAPE_REPRESENTATION(#68,#4836);
#97=CONTEXT_DEPENDENT_SHAPE_REPRESENTATION(#69,#4837);
#98=CONTEXT_DEPENDENT_SHAPE_REPRESENTATION(#70,#4838);
#99=CONTEXT_DEPENDENT_SHAPE_REPRESENTATION(#71,#4839);
#100=CONTEXT_DEPENDENT_SHAPE_REPRESENTATION(#72,#4840);
#101=CONTEXT_DEPENDENT_SHAPE_REPRESENTATION(#73,#4841);
#102=CONTEXT_DEPENDENT_SHAPE_REPRESENTATION(#74,#4842);
#103=CONTEXT_DEPENDENT_SHAPE_REPRESENTATION(#75,#4843);
#104=CONTEXT_DEPENDENT_SHAPE_REPRESENTATION(#76,#4844);
#105=CONTEXT_DEPENDENT_SHAPE_REPRESENTATION(#77,#4845);
#106=CONTEXT_DEPENDENT_SHAPE_REPRESENTATION(#78,#4846);
#107=CONTEXT_DEPENDENT_SHAPE_REPRESENTATION(#79,#4847);
#108=CONTEXT_DEPENDENT_SHAPE_REPRESENTATION(#80,#4848);
#109=CONTEXT_DEPENDENT_SHAPE_REPRESENTATION(#81,#4849);
#110=CONTEXT_DEPENDENT_SHAPE_REPRESENTATION(#82,#4850);
#111=CONTEXT_DEPENDENT_SHAPE_REPRESENTATION(#83,#4851);
#112=CONTEXT_DEPENDENT_SHAPE_REPRESENTATION(#84,#4852);
#113=CONTEXT_DEPENDENT_SHAPE_REPRESENTATION(#85,#4853);
#114=CONTEXT_DEPENDENT_SHAPE_REPRESENTATION(#86,#4854);
#115=CONTEXT_DEPENDENT_SHAPE_REPRESENTATION(#87,#4855);
#116=CONTEXT_DEPENDENT_SHAPE_REPRESENTATION(#88,#4856);
#117=CONTEXT_DEPENDENT_SHAPE_REPRESENTATION(#89,#4857);
#118=CONTEXT_DEPENDENT_SHAPE_REPRESENTATION(#90,#4858);
#119=CONTEXT_DEPENDENT_SHAPE_REPRESENTATION(#91,#4859);
#120=NEXT_ASSEMBLY_USAGE_OCCURRENCE(
'Thirty-five millimetre toggle link:1',
'Thirty-five millimetre toggle link:1',
'Thirty-five millimetre toggle link:1',#4886,#4887,
'Thirty-five millimetre toggle link:1');
#121=NEXT_ASSEMBLY_USAGE_OCCURRENCE(
'Twenty-five millimetre clamp base:1',
'Twenty-five millimetre clamp base:1',
'Twenty-five millimetre clamp base:1',#4880,#4881,
'Twenty-five millimetre clamp base:1');
#122=NEXT_ASSEMBLY_USAGE_OCCURRENCE('Pivot retention spacer:1',
'Pivot retention spacer:1','Pivot retention spacer:1',#4880,#4895,
'Pivot retention spacer:1');
#123=NEXT_ASSEMBLY_USAGE_OCCURRENCE('Clevis Pin - 6x30:2',
'Clevis Pin - 6x30:2','Clevis Pin - 6x30:2',#4880,#4893,
'Clevis Pin - 6x30:2');
#124=NEXT_ASSEMBLY_USAGE_OCCURRENCE('Flat Washer - M6:2',
'Flat Washer - M6:2','Flat Washer - M6:2',#4880,#4894,
'Flat Washer - M6:2');
#125=NEXT_ASSEMBLY_USAGE_OCCURRENCE('Flat Washer - M6:3',
'Flat Washer - M6:3','Flat Washer - M6:3',#4880,#4894,
'Flat Washer - M6:3');
#126=NEXT_ASSEMBLY_USAGE_OCCURRENCE('Split Pin - 1.6x16:2',
'Split Pin - 1.6x16:2','Split Pin - 1.6x16:2',#4880,#4896,
'Split Pin - 1.6x16:2');
#127=NEXT_ASSEMBLY_USAGE_OCCURRENCE('Operating lever:1',
'Operating lever:1','Operating lever:1',#4882,#4883,'Operating lever:1');
#128=NEXT_ASSEMBLY_USAGE_OCCURRENCE('Handle:2','Handle:2','Handle:2',#4882,
#4884,'Handle:2');
#129=NEXT_ASSEMBLY_USAGE_OCCURRENCE('M5x14 Cap Screw:2',
'M5x14 Cap Screw:2','M5x14 Cap Screw:2',#4882,#4885,'M5x14 Cap Screw:2');
#130=NEXT_ASSEMBLY_USAGE_OCCURRENCE('Clevis Pin - 6x30:3',
'Clevis Pin - 6x30:3','Clevis Pin - 6x30:3',#4882,#4893,
'Clevis Pin - 6x30:3');
#131=NEXT_ASSEMBLY_USAGE_OCCURRENCE('Flat Washer - M6:4',
'Flat Washer - M6:4','Flat Washer - M6:4',#4882,#4894,
'Flat Washer - M6:4');
#132=NEXT_ASSEMBLY_USAGE_OCCURRENCE('Flat Washer - M6:5',
'Flat Washer - M6:5','Flat Washer - M6:5',#4882,#4894,
'Flat Washer - M6:5');
#133=NEXT_ASSEMBLY_USAGE_OCCURRENCE('Pivot retention spacer:2',
'Pivot retention spacer:2','Pivot retention spacer:2',#4882,#4895,
'Pivot retention spacer:2');
#134=NEXT_ASSEMBLY_USAGE_OCCURRENCE('Split Pin - 1.6x16:3',
'Split Pin - 1.6x16:3','Split Pin - 1.6x16:3',#4882,#4896,
'Split Pin - 1.6x16:3');
#135=NEXT_ASSEMBLY_USAGE_OCCURRENCE('Forked pressure plunger:1',
'Forked pressure plunger:1','Forked pressure plunger:1',#4888,#4889,
'Forked pressure plunger:1');
#136=NEXT_ASSEMBLY_USAGE_OCCURRENCE('Hex Bolt - M8x40:2',
'Hex Bolt - M8x40:2','Hex Bolt - M8x40:2',#4888,#4890,
'Hex Bolt - M8x40:2');
#137=NEXT_ASSEMBLY_USAGE_OCCURRENCE('Hex Nut - M8:2','Hex Nut - M8:2',
'Hex Nut - M8:2',#4888,#4891,'Hex Nut - M8:2');
#138=NEXT_ASSEMBLY_USAGE_OCCURRENCE(
'Elastomer pressure pad installed:2',
'Elastomer pressure pad installed:2',
'Elastomer pressure pad installed:2',#4888,#4892,
'Elastomer pressure pad installed:2');
#139=NEXT_ASSEMBLY_USAGE_OCCURRENCE('Clevis Pin - 6x30:4',
'Clevis Pin - 6x30:4','Clevis Pin - 6x30:4',#4888,#4893,
'Clevis Pin - 6x30:4');
#140=NEXT_ASSEMBLY_USAGE_OCCURRENCE('Flat Washer - M6:6',
'Flat Washer - M6:6','Flat Washer - M6:6',#4888,#4894,
'Flat Washer - M6:6');
#141=NEXT_ASSEMBLY_USAGE_OCCURRENCE('Flat Washer - M6:7',
'Flat Washer - M6:7','Flat Washer - M6:7',#4888,#4894,
'Flat Washer - M6:7');
#142=NEXT_ASSEMBLY_USAGE_OCCURRENCE('Pivot retention spacer:3',
'Pivot retention spacer:3','Pivot retention spacer:3',#4888,#4895,
'Pivot retention spacer:3');
#143=NEXT_ASSEMBLY_USAGE_OCCURRENCE('Split Pin - 1.6x16:4',
'Split Pin - 1.6x16:4','Split Pin - 1.6x16:4',#4888,#4896,
'Split Pin - 1.6x16:4');
#144=NEXT_ASSEMBLY_USAGE_OCCURRENCE('Base guide and handle stop:1',
'Base guide and handle stop:1','Base guide and handle stop:1',#4879,#4880,
'Base guide and handle stop:1');
#145=NEXT_ASSEMBLY_USAGE_OCCURRENCE('Operating crank:1',
'Operating crank:1','Operating crank:1',#4879,#4882,'Operating crank:1');
#146=NEXT_ASSEMBLY_USAGE_OCCURRENCE('Toggle connecting link:1',
'Toggle connecting link:1','Toggle connecting link:1',#4879,#4886,
'Toggle connecting link:1');
#147=NEXT_ASSEMBLY_USAGE_OCCURRENCE('Plunger and M8 spindle:1',
'Plunger and M8 spindle:1','Plunger and M8 spindle:1',#4879,#4888,
'Plunger and M8 spindle:1');
#148=CONICAL_SURFACE('',#2904,0.4,0.785398163397448);
#149=CONICAL_SURFACE('',#2908,0.41,0.785398163397448);
#150=CONICAL_SURFACE('',#2912,0.26,0.463647609000806);
#151=CONICAL_SURFACE('',#2964,0.36,0.785398163397451);
#152=CONICAL_SURFACE('',#2967,0.734027674973257,1.0471975511966);
#153=CONICAL_SURFACE('',#2978,0.734027674973257,1.0471975511966);
#154=CONICAL_SURFACE('',#2980,0.734027674973257,1.0471975511966);
#155=CONICAL_SURFACE('',#3003,0.475,0.785398163397448);
#156=CONICAL_SURFACE('',#3011,0.255,0.785398163397449);
#157=ORIENTED_CLOSED_SHELL('',*,#2632,.F.);
#158=BREP_WITH_VOIDS('Body1',#2633,(#157));
#159=SHAPE_REPRESENTATION_RELATIONSHIP('SRR','None',#4862,#172);
#160=SHAPE_REPRESENTATION_RELATIONSHIP('SRR','None',#4864,#173);
#161=SHAPE_REPRESENTATION_RELATIONSHIP('SRR','None',#4865,#174);
#162=SHAPE_REPRESENTATION_RELATIONSHIP('SRR','None',#4866,#175);
#163=SHAPE_REPRESENTATION_RELATIONSHIP('SRR','None',#4868,#176);
#164=SHAPE_REPRESENTATION_RELATIONSHIP('SRR','None',#4870,#177);
#165=SHAPE_REPRESENTATION_RELATIONSHIP('SRR','None',#4871,#178);
#166=SHAPE_REPRESENTATION_RELATIONSHIP('SRR','None',#4872,#179);
#167=SHAPE_REPRESENTATION_RELATIONSHIP('SRR','None',#4873,#180);
#168=SHAPE_REPRESENTATION_RELATIONSHIP('SRR','None',#4874,#181);
#169=SHAPE_REPRESENTATION_RELATIONSHIP('SRR','None',#4875,#182);
#170=SHAPE_REPRESENTATION_RELATIONSHIP('SRR','None',#4876,#183);
#171=SHAPE_REPRESENTATION_RELATIONSHIP('SRR','None',#4877,#184);
#172=ADVANCED_BREP_SHAPE_REPRESENTATION('',(#198),#4775);
#173=ADVANCED_BREP_SHAPE_REPRESENTATION('',(#199),#4777);
#174=ADVANCED_BREP_SHAPE_REPRESENTATION('',(#200),#4778);
#175=ADVANCED_BREP_SHAPE_REPRESENTATION('',(#158),#4779);
#176=ADVANCED_BREP_SHAPE_REPRESENTATION('',(#201),#4781);
#177=ADVANCED_BREP_SHAPE_REPRESENTATION('',(#202),#4783);
#178=ADVANCED_BREP_SHAPE_REPRESENTATION('',(#203),#4784);
#179=ADVANCED_BREP_SHAPE_REPRESENTATION('',(#204),#4785);
#180=ADVANCED_BREP_SHAPE_REPRESENTATION('',(#205),#4786);
#181=ADVANCED_BREP_SHAPE_REPRESENTATION('',(#206),#4787);
#182=ADVANCED_BREP_SHAPE_REPRESENTATION('',(#207),#4788);
#183=ADVANCED_BREP_SHAPE_REPRESENTATION('',(#208),#4789);
#184=ADVANCED_BREP_SHAPE_REPRESENTATION('',(#209),#4790);
#185=STYLED_ITEM('',(#5002),#198);
#186=STYLED_ITEM('',(#5009),#199);
#187=STYLED_ITEM('',(#5016),#200);
#188=STYLED_ITEM('',(#5030),#158);
#189=STYLED_ITEM('',(#5037),#201);
#190=STYLED_ITEM('',(#5009),#202);
#191=STYLED_ITEM('',(#5030),#203);
#192=STYLED_ITEM('',(#5030),#204);
#193=STYLED_ITEM('',(#5037),#205);
#194=STYLED_ITEM('',(#5023),#206);
#195=STYLED_ITEM('',(#5030),#207);
#196=STYLED_ITEM('',(#5037),#208);
#197=STYLED_ITEM('',(#5023),#209);
#198=MANIFOLD_SOLID_BREP('Body1',#2629);
#199=MANIFOLD_SOLID_BREP('Body1',#2630);
#200=MANIFOLD_SOLID_BREP('Body1',#2631);
#201=MANIFOLD_SOLID_BREP('Body1',#2634);
#202=MANIFOLD_SOLID_BREP('Body1',#2635);
#203=MANIFOLD_SOLID_BREP('Body1',#2636);
#204=MANIFOLD_SOLID_BREP('Body1',#2637);
#205=MANIFOLD_SOLID_BREP('Body1',#2638);
#206=MANIFOLD_SOLID_BREP('Body1',#2639);
#207=MANIFOLD_SOLID_BREP('Body1',#2640);
#208=MANIFOLD_SOLID_BREP('Body1',#2641);
#209=MANIFOLD_SOLID_BREP('Body1',#2642);
#210=FACE_BOUND('',#522,.T.);
#211=FACE_BOUND('',#523,.T.);
#212=FACE_BOUND('',#524,.T.);
#213=FACE_BOUND('',#525,.T.);
#214=FACE_BOUND('',#526,.T.);
#215=FACE_BOUND('',#532,.T.);
#216=FACE_BOUND('',#534,.T.);
#217=FACE_BOUND('',#540,.T.);
#218=FACE_BOUND('',#545,.T.);
#219=FACE_BOUND('',#547,.T.);
#220=FACE_BOUND('',#552,.T.);
#221=FACE_BOUND('',#557,.T.);
#222=FACE_BOUND('',#558,.T.);
#223=FACE_BOUND('',#563,.T.);
#224=FACE_BOUND('',#566,.T.);
#225=FACE_BOUND('',#572,.T.);
#226=FACE_BOUND('',#575,.T.);
#227=FACE_BOUND('',#581,.T.);
#228=FACE_BOUND('',#582,.T.);
#229=FACE_BOUND('',#584,.T.);
#230=FACE_BOUND('',#586,.T.);
#231=FACE_BOUND('',#589,.T.);
#232=FACE_BOUND('',#591,.T.);
#233=FACE_BOUND('',#595,.T.);
#234=FACE_BOUND('',#600,.T.);
#235=FACE_BOUND('',#616,.T.);
#236=FACE_BOUND('',#624,.T.);
#237=FACE_BOUND('',#625,.T.);
#238=FACE_BOUND('',#629,.T.);
#239=FACE_BOUND('',#630,.T.);
#240=FACE_BOUND('',#637,.T.);
#241=FACE_BOUND('',#640,.T.);
#242=FACE_BOUND('',#643,.T.);
#243=FACE_BOUND('',#646,.T.);
#244=FACE_BOUND('',#649,.T.);
#245=FACE_BOUND('',#652,.T.);
#246=FACE_BOUND('',#665,.T.);
#247=FACE_BOUND('',#676,.T.);
#248=FACE_BOUND('',#678,.T.);
#249=FACE_BOUND('',#687,.T.);
#250=FACE_BOUND('',#689,.T.);
#251=FACE_BOUND('',#695,.T.);
#252=FACE_BOUND('',#697,.T.);
#253=FACE_BOUND('',#701,.T.);
#254=FACE_BOUND('',#703,.T.);
#255=FACE_BOUND('',#705,.T.);
#256=PLANE('',#2795);
#257=PLANE('',#2796);
#258=PLANE('',#2797);
#259=PLANE('',#2798);
#260=PLANE('',#2799);
#261=PLANE('',#2800);
#262=PLANE('',#2801);
#263=PLANE('',#2802);
#264=PLANE('',#2812);
#265=PLANE('',#2813);
#266=PLANE('',#2814);
#267=PLANE('',#2815);
#268=PLANE('',#2816);
#269=PLANE('',#2823);
#270=PLANE('',#2824);
#271=PLANE('',#2825);
#272=PLANE('',#2826);
#273=PLANE('',#2827);
#274=PLANE('',#2828);
#275=PLANE('',#2829);
#276=PLANE('',#2830);
#277=PLANE('',#2831);
#278=PLANE('',#2832);
#279=PLANE('',#2833);
#280=PLANE('',#2834);
#281=PLANE('',#2835);
#282=PLANE('',#2836);
#283=PLANE('',#2848);
#284=PLANE('',#2850);
#285=PLANE('',#2851);
#286=PLANE('',#2853);
#287=PLANE('',#2860);
#288=PLANE('',#2861);
#289=PLANE('',#2862);
#290=PLANE('',#2863);
#291=PLANE('',#2864);
#292=PLANE('',#2866);
#293=PLANE('',#2867);
#294=PLANE('',#2869);
#295=PLANE('',#2873);
#296=PLANE('',#2874);
#297=PLANE('',#2875);
#298=PLANE('',#2876);
#299=PLANE('',#2877);
#300=PLANE('',#2878);
#301=PLANE('',#2879);
#302=PLANE('',#2880);
#303=PLANE('',#2885);
#304=PLANE('',#2889);
#305=PLANE('',#2890);
#306=PLANE('',#2892);
#307=PLANE('',#2893);
#308=PLANE('',#2894);
#309=PLANE('',#2895);
#310=PLANE('',#2896);
#311=PLANE('',#2897);
#312=PLANE('',#2898);
#313=PLANE('',#2899);
#314=PLANE('',#2900);
#315=PLANE('',#2902);
#316=PLANE('',#2910);
#317=PLANE('',#2926);
#318=PLANE('',#2927);
#319=PLANE('',#2929);
#320=PLANE('',#2932);
#321=PLANE('',#2939);
#322=PLANE('',#2946);
#323=PLANE('',#2947);
#324=PLANE('',#2948);
#325=PLANE('',#2949);
#326=PLANE('',#2950);
#327=PLANE('',#2951);
#328=PLANE('',#2953);
#329=PLANE('',#2954);
#330=PLANE('',#2955);
#331=PLANE('',#2956);
#332=PLANE('',#2959);
#333=PLANE('',#2966);
#334=PLANE('',#2969);
#335=PLANE('',#2970);
#336=PLANE('',#2971);
#337=PLANE('',#2972);
#338=PLANE('',#2973);
#339=PLANE('',#2974);
#340=PLANE('',#2975);
#341=PLANE('',#2976);
#342=PLANE('',#2982);
#343=PLANE('',#2983);
#344=PLANE('',#2984);
#345=PLANE('',#2988);
#346=PLANE('',#2989);
#347=PLANE('',#2990);
#348=PLANE('',#2991);
#349=PLANE('',#2992);
#350=PLANE('',#2997);
#351=PLANE('',#2998);
#352=PLANE('',#3001);
#353=PLANE('',#3007);
#354=PLANE('',#3013);
#355=PLANE('',#3021);
#356=PLANE('',#3022);
#357=PLANE('',#3030);
#358=PLANE('',#3031);
#359=PLANE('',#3036);
#360=PLANE('',#3038);
#361=PLANE('',#3042);
#362=FACE_OUTER_BOUND('',#513,.T.);
#363=FACE_OUTER_BOUND('',#514,.T.);
#364=FACE_OUTER_BOUND('',#515,.T.);
#365=FACE_OUTER_BOUND('',#516,.T.);
#366=FACE_OUTER_BOUND('',#517,.T.);
#367=FACE_OUTER_BOUND('',#518,.T.);
#368=FACE_OUTER_BOUND('',#519,.T.);
#369=FACE_OUTER_BOUND('',#520,.T.);
#370=FACE_OUTER_BOUND('',#521,.T.);
#371=FACE_OUTER_BOUND('',#527,.T.);
#372=FACE_OUTER_BOUND('',#528,.T.);
#373=FACE_OUTER_BOUND('',#529,.T.);
#374=FACE_OUTER_BOUND('',#530,.T.);
#375=FACE_OUTER_BOUND('',#531,.T.);
#376=FACE_OUTER_BOUND('',#533,.T.);
#377=FACE_OUTER_BOUND('',#535,.T.);
#378=FACE_OUTER_BOUND('',#536,.T.);
#379=FACE_OUTER_BOUND('',#537,.T.);
#380=FACE_OUTER_BOUND('',#538,.T.);
#381=FACE_OUTER_BOUND('',#539,.T.);
#382=FACE_OUTER_BOUND('',#541,.T.);
#383=FACE_OUTER_BOUND('',#542,.T.);
#384=FACE_OUTER_BOUND('',#543,.T.);
#385=FACE_OUTER_BOUND('',#544,.T.);
#386=FACE_OUTER_BOUND('',#546,.T.);
#387=FACE_OUTER_BOUND('',#548,.T.);
#388=FACE_OUTER_BOUND('',#549,.T.);
#389=FACE_OUTER_BOUND('',#550,.T.);
#390=FACE_OUTER_BOUND('',#551,.T.);
#391=FACE_OUTER_BOUND('',#553,.T.);
#392=FACE_OUTER_BOUND('',#554,.T.);
#393=FACE_OUTER_BOUND('',#555,.T.);
#394=FACE_OUTER_BOUND('',#556,.T.);
#395=FACE_OUTER_BOUND('',#559,.T.);
#396=FACE_OUTER_BOUND('',#560,.T.);
#397=FACE_OUTER_BOUND('',#561,.T.);
#398=FACE_OUTER_BOUND('',#562,.T.);
#399=FACE_OUTER_BOUND('',#564,.T.);
#400=FACE_OUTER_BOUND('',#565,.T.);
#401=FACE_OUTER_BOUND('',#567,.T.);
#402=FACE_OUTER_BOUND('',#568,.T.);
#403=FACE_OUTER_BOUND('',#569,.T.);
#404=FACE_OUTER_BOUND('',#570,.T.);
#405=FACE_OUTER_BOUND('',#571,.T.);
#406=FACE_OUTER_BOUND('',#573,.T.);
#407=FACE_OUTER_BOUND('',#574,.T.);
#408=FACE_OUTER_BOUND('',#576,.T.);
#409=FACE_OUTER_BOUND('',#577,.T.);
#410=FACE_OUTER_BOUND('',#578,.T.);
#411=FACE_OUTER_BOUND('',#579,.T.);
#412=FACE_OUTER_BOUND('',#580,.T.);
#413=FACE_OUTER_BOUND('',#583,.T.);
#414=FACE_OUTER_BOUND('',#585,.T.);
#415=FACE_OUTER_BOUND('',#587,.T.);
#416=FACE_OUTER_BOUND('',#588,.T.);
#417=FACE_OUTER_BOUND('',#590,.T.);
#418=FACE_OUTER_BOUND('',#592,.T.);
#419=FACE_OUTER_BOUND('',#593,.T.);
#420=FACE_OUTER_BOUND('',#594,.T.);
#421=FACE_OUTER_BOUND('',#596,.T.);
#422=FACE_OUTER_BOUND('',#597,.T.);
#423=FACE_OUTER_BOUND('',#598,.T.);
#424=FACE_OUTER_BOUND('',#599,.T.);
#425=FACE_OUTER_BOUND('',#601,.T.);
#426=FACE_OUTER_BOUND('',#602,.T.);
#427=FACE_OUTER_BOUND('',#603,.T.);
#428=FACE_OUTER_BOUND('',#604,.T.);
#429=FACE_OUTER_BOUND('',#605,.T.);
#430=FACE_OUTER_BOUND('',#606,.T.);
#431=FACE_OUTER_BOUND('',#607,.T.);
#432=FACE_OUTER_BOUND('',#608,.T.);
#433=FACE_OUTER_BOUND('',#609,.T.);
#434=FACE_OUTER_BOUND('',#610,.T.);
#435=FACE_OUTER_BOUND('',#611,.T.);
#436=FACE_OUTER_BOUND('',#612,.T.);
#437=FACE_OUTER_BOUND('',#613,.T.);
#438=FACE_OUTER_BOUND('',#614,.T.);
#439=FACE_OUTER_BOUND('',#615,.T.);
#440=FACE_OUTER_BOUND('',#617,.T.);
#441=FACE_OUTER_BOUND('',#618,.T.);
#442=FACE_OUTER_BOUND('',#619,.T.);
#443=FACE_OUTER_BOUND('',#620,.T.);
#444=FACE_OUTER_BOUND('',#621,.T.);
#445=FACE_OUTER_BOUND('',#622,.T.);
#446=FACE_OUTER_BOUND('',#623,.T.);
#447=FACE_OUTER_BOUND('',#626,.T.);
#448=FACE_OUTER_BOUND('',#627,.T.);
#449=FACE_OUTER_BOUND('',#628,.T.);
#450=FACE_OUTER_BOUND('',#631,.T.);
#451=FACE_OUTER_BOUND('',#632,.T.);
#452=FACE_OUTER_BOUND('',#633,.T.);
#453=FACE_OUTER_BOUND('',#634,.T.);
#454=FACE_OUTER_BOUND('',#635,.T.);
#455=FACE_OUTER_BOUND('',#636,.T.);
#456=FACE_OUTER_BOUND('',#638,.T.);
#457=FACE_OUTER_BOUND('',#639,.T.);
#458=FACE_OUTER_BOUND('',#641,.T.);
#459=FACE_OUTER_BOUND('',#642,.T.);
#460=FACE_OUTER_BOUND('',#644,.T.);
#461=FACE_OUTER_BOUND('',#645,.T.);
#462=FACE_OUTER_BOUND('',#647,.T.);
#463=FACE_OUTER_BOUND('',#648,.T.);
#464=FACE_OUTER_BOUND('',#650,.T.);
#465=FACE_OUTER_BOUND('',#651,.T.);
#466=FACE_OUTER_BOUND('',#653,.T.);
#467=FACE_OUTER_BOUND('',#654,.T.);
#468=FACE_OUTER_BOUND('',#655,.T.);
#469=FACE_OUTER_BOUND('',#656,.T.);
#470=FACE_OUTER_BOUND('',#657,.T.);
#471=FACE_OUTER_BOUND('',#658,.T.);
#472=FACE_OUTER_BOUND('',#659,.T.);
#473=FACE_OUTER_BOUND('',#660,.T.);
#474=FACE_OUTER_BOUND('',#661,.T.);
#475=FACE_OUTER_BOUND('',#662,.T.);
#476=FACE_OUTER_BOUND('',#663,.T.);
#477=FACE_OUTER_BOUND('',#664,.T.);
#478=FACE_OUTER_BOUND('',#666,.T.);
#479=FACE_OUTER_BOUND('',#667,.T.);
#480=FACE_OUTER_BOUND('',#668,.T.);
#481=FACE_OUTER_BOUND('',#669,.T.);
#482=FACE_OUTER_BOUND('',#670,.T.);
#483=FACE_OUTER_BOUND('',#671,.T.);
#484=FACE_OUTER_BOUND('',#672,.T.);
#485=FACE_OUTER_BOUND('',#673,.T.);
#486=FACE_OUTER_BOUND('',#674,.T.);
#487=FACE_OUTER_BOUND('',#675,.T.);
#488=FACE_OUTER_BOUND('',#677,.T.);
#489=FACE_OUTER_BOUND('',#679,.T.);
#490=FACE_OUTER_BOUND('',#680,.T.);
#491=FACE_OUTER_BOUND('',#681,.T.);
#492=FACE_OUTER_BOUND('',#682,.T.);
#493=FACE_OUTER_BOUND('',#683,.T.);
#494=FACE_OUTER_BOUND('',#684,.T.);
#495=FACE_OUTER_BOUND('',#685,.T.);
#496=FACE_OUTER_BOUND('',#686,.T.);
#497=FACE_OUTER_BOUND('',#688,.T.);
#498=FACE_OUTER_BOUND('',#690,.T.);
#499=FACE_OUTER_BOUND('',#691,.T.);
#500=FACE_OUTER_BOUND('',#692,.T.);
#501=FACE_OUTER_BOUND('',#693,.T.);
#502=FACE_OUTER_BOUND('',#694,.T.);
#503=FACE_OUTER_BOUND('',#696,.T.);
#504=FACE_OUTER_BOUND('',#698,.T.);
#505=FACE_OUTER_BOUND('',#699,.T.);
#506=FACE_OUTER_BOUND('',#700,.T.);
#507=FACE_OUTER_BOUND('',#702,.T.);
#508=FACE_OUTER_BOUND('',#704,.T.);
#509=FACE_OUTER_BOUND('',#706,.T.);
#510=FACE_OUTER_BOUND('',#707,.T.);
#511=FACE_OUTER_BOUND('',#708,.T.);
#512=FACE_OUTER_BOUND('',#709,.T.);
#513=EDGE_LOOP('',(#1783,#1784,#1785,#1786,#1787,#1788,#1789,#1790));
#514=EDGE_LOOP('',(#1791));
#515=EDGE_LOOP('',(#1792,#1793,#1794,#1795,#1796,#1797,#1798,#1799,#1800,
#1801,#1802));
#516=EDGE_LOOP('',(#1803,#1804,#1805,#1806));
#517=EDGE_LOOP('',(#1807,#1808,#1809,#1810));
#518=EDGE_LOOP('',(#1811,#1812,#1813,#1814));
#519=EDGE_LOOP('',(#1815,#1816,#1817,#1818));
#520=EDGE_LOOP('',(#1819,#1820,#1821,#1822,#1823,#1824));
#521=EDGE_LOOP('',(#1825,#1826,#1827,#1828,#1829,#1830,#1831,#1832));
#522=EDGE_LOOP('',(#1833,#1834,#1835,#1836));
#523=EDGE_LOOP('',(#1837,#1838,#1839,#1840));
#524=EDGE_LOOP('',(#1841,#1842,#1843,#1844));
#525=EDGE_LOOP('',(#1845));
#526=EDGE_LOOP('',(#1846));
#527=EDGE_LOOP('',(#1847,#1848,#1849,#1850));
#528=EDGE_LOOP('',(#1851,#1852,#1853,#1854));
#529=EDGE_LOOP('',(#1855,#1856,#1857,#1858));
#530=EDGE_LOOP('',(#1859,#1860,#1861,#1862));
#531=EDGE_LOOP('',(#1863,#1864,#1865,#1866));
#532=EDGE_LOOP('',(#1867));
#533=EDGE_LOOP('',(#1868,#1869,#1870,#1871));
#534=EDGE_LOOP('',(#1872));
#535=EDGE_LOOP('',(#1873,#1874,#1875,#1876));
#536=EDGE_LOOP('',(#1877,#1878,#1879,#1880));
#537=EDGE_LOOP('',(#1881,#1882,#1883,#1884));
#538=EDGE_LOOP('',(#1885,#1886,#1887,#1888));
#539=EDGE_LOOP('',(#1889,#1890,#1891,#1892));
#540=EDGE_LOOP('',(#1893));
#541=EDGE_LOOP('',(#1894,#1895,#1896,#1897));
#542=EDGE_LOOP('',(#1898,#1899,#1900,#1901));
#543=EDGE_LOOP('',(#1902,#1903,#1904,#1905));
#544=EDGE_LOOP('',(#1906,#1907,#1908,#1909));
#545=EDGE_LOOP('',(#1910));
#546=EDGE_LOOP('',(#1911,#1912,#1913,#1914));
#547=EDGE_LOOP('',(#1915));
#548=EDGE_LOOP('',(#1916,#1917,#1918,#1919));
#549=EDGE_LOOP('',(#1920,#1921,#1922,#1923));
#550=EDGE_LOOP('',(#1924,#1925,#1926,#1927));
#551=EDGE_LOOP('',(#1928,#1929,#1930,#1931));
#552=EDGE_LOOP('',(#1932));
#553=EDGE_LOOP('',(#1933,#1934,#1935,#1936));
#554=EDGE_LOOP('',(#1937,#1938,#1939,#1940));
#555=EDGE_LOOP('',(#1941,#1942,#1943,#1944));
#556=EDGE_LOOP('',(#1945,#1946,#1947,#1948));
#557=EDGE_LOOP('',(#1949));
#558=EDGE_LOOP('',(#1950));
#559=EDGE_LOOP('',(#1951,#1952,#1953,#1954));
#560=EDGE_LOOP('',(#1955,#1956,#1957,#1958));
#561=EDGE_LOOP('',(#1959,#1960,#1961,#1962));
#562=EDGE_LOOP('',(#1963,#1964,#1965,#1966));
#563=EDGE_LOOP('',(#1967));
#564=EDGE_LOOP('',(#1968,#1969,#1970,#1971));
#565=EDGE_LOOP('',(#1972,#1973,#1974,#1975));
#566=EDGE_LOOP('',(#1976));
#567=EDGE_LOOP('',(#1977,#1978,#1979,#1980));
#568=EDGE_LOOP('',(#1981,#1982,#1983,#1984));
#569=EDGE_LOOP('',(#1985,#1986,#1987,#1988));
#570=EDGE_LOOP('',(#1989,#1990,#1991,#1992));
#571=EDGE_LOOP('',(#1993,#1994,#1995,#1996));
#572=EDGE_LOOP('',(#1997));
#573=EDGE_LOOP('',(#1998,#1999,#2000,#2001));
#574=EDGE_LOOP('',(#2002,#2003,#2004,#2005));
#575=EDGE_LOOP('',(#2006));
#576=EDGE_LOOP('',(#2007,#2008,#2009,#2010));
#577=EDGE_LOOP('',(#2011,#2012,#2013,#2014));
#578=EDGE_LOOP('',(#2015,#2016,#2017,#2018));
#579=EDGE_LOOP('',(#2019,#2020,#2021,#2022));
#580=EDGE_LOOP('',(#2023,#2024,#2025,#2026));
#581=EDGE_LOOP('',(#2027,#2028,#2029,#2030));
#582=EDGE_LOOP('',(#2031,#2032,#2033,#2034));
#583=EDGE_LOOP('',(#2035));
#584=EDGE_LOOP('',(#2036));
#585=EDGE_LOOP('',(#2037));
#586=EDGE_LOOP('',(#2038));
#587=EDGE_LOOP('',(#2039,#2040,#2041,#2042,#2043,#2044,#2045,#2046));
#588=EDGE_LOOP('',(#2047,#2048,#2049,#2050));
#589=EDGE_LOOP('',(#2051));
#590=EDGE_LOOP('',(#2052,#2053,#2054,#2055));
#591=EDGE_LOOP('',(#2056,#2057,#2058,#2059));
#592=EDGE_LOOP('',(#2060,#2061,#2062,#2063));
#593=EDGE_LOOP('',(#2064,#2065,#2066,#2067,#2068,#2069,#2070,#2071));
#594=EDGE_LOOP('',(#2072,#2073,#2074,#2075));
#595=EDGE_LOOP('',(#2076));
#596=EDGE_LOOP('',(#2077,#2078,#2079,#2080));
#597=EDGE_LOOP('',(#2081));
#598=EDGE_LOOP('',(#2082,#2083,#2084,#2085));
#599=EDGE_LOOP('',(#2086));
#600=EDGE_LOOP('',(#2087));
#601=EDGE_LOOP('',(#2088));
#602=EDGE_LOOP('',(#2089,#2090,#2091,#2092));
#603=EDGE_LOOP('',(#2093,#2094,#2095,#2096));
#604=EDGE_LOOP('',(#2097,#2098,#2099,#2100));
#605=EDGE_LOOP('',(#2101,#2102,#2103,#2104));
#606=EDGE_LOOP('',(#2105,#2106,#2107,#2108));
#607=EDGE_LOOP('',(#2109,#2110,#2111,#2112));
#608=EDGE_LOOP('',(#2113,#2114,#2115,#2116,#2117,#2118));
#609=EDGE_LOOP('',(#2119,#2120,#2121,#2122,#2123,#2124));
#610=EDGE_LOOP('',(#2125));
#611=EDGE_LOOP('',(#2126));
#612=EDGE_LOOP('',(#2127,#2128,#2129,#2130));
#613=EDGE_LOOP('',(#2131,#2132,#2133,#2134));
#614=EDGE_LOOP('',(#2135,#2136,#2137,#2138));
#615=EDGE_LOOP('',(#2139));
#616=EDGE_LOOP('',(#2140));
#617=EDGE_LOOP('',(#2141,#2142,#2143,#2144));
#618=EDGE_LOOP('',(#2145,#2146,#2147,#2148));
#619=EDGE_LOOP('',(#2149,#2150,#2151,#2152));
#620=EDGE_LOOP('',(#2153,#2154,#2155,#2156));
#621=EDGE_LOOP('',(#2157,#2158,#2159,#2160));
#622=EDGE_LOOP('',(#2161,#2162,#2163,#2164));
#623=EDGE_LOOP('',(#2165,#2166,#2167,#2168));
#624=EDGE_LOOP('',(#2169));
#625=EDGE_LOOP('',(#2170));
#626=EDGE_LOOP('',(#2171,#2172,#2173,#2174));
#627=EDGE_LOOP('',(#2175,#2176,#2177,#2178));
#628=EDGE_LOOP('',(#2179,#2180,#2181,#2182));
#629=EDGE_LOOP('',(#2183));
#630=EDGE_LOOP('',(#2184));
#631=EDGE_LOOP('',(#2185,#2186,#2187,#2188));
#632=EDGE_LOOP('',(#2189));
#633=EDGE_LOOP('',(#2190,#2191,#2192,#2193));
#634=EDGE_LOOP('',(#2194,#2195,#2196,#2197));
#635=EDGE_LOOP('',(#2198,#2199,#2200,#2201));
#636=EDGE_LOOP('',(#2202,#2203,#2204,#2205));
#637=EDGE_LOOP('',(#2206));
#638=EDGE_LOOP('',(#2207,#2208,#2209,#2210,#2211,#2212,#2213,#2214));
#639=EDGE_LOOP('',(#2215,#2216,#2217,#2218));
#640=EDGE_LOOP('',(#2219));
#641=EDGE_LOOP('',(#2220,#2221,#2222,#2223));
#642=EDGE_LOOP('',(#2224,#2225,#2226,#2227));
#643=EDGE_LOOP('',(#2228));
#644=EDGE_LOOP('',(#2229,#2230,#2231,#2232,#2233,#2234,#2235,#2236));
#645=EDGE_LOOP('',(#2237,#2238,#2239,#2240));
#646=EDGE_LOOP('',(#2241));
#647=EDGE_LOOP('',(#2242,#2243,#2244,#2245));
#648=EDGE_LOOP('',(#2246,#2247,#2248,#2249));
#649=EDGE_LOOP('',(#2250));
#650=EDGE_LOOP('',(#2251,#2252,#2253,#2254));
#651=EDGE_LOOP('',(#2255));
#652=EDGE_LOOP('',(#2256));
#653=EDGE_LOOP('',(#2257,#2258,#2259,#2260));
#654=EDGE_LOOP('',(#2261,#2262,#2263,#2264));
#655=EDGE_LOOP('',(#2265));
#656=EDGE_LOOP('',(#2266,#2267,#2268,#2269,#2270,#2271,#2272,#2273,#2274));
#657=EDGE_LOOP('',(#2275,#2276,#2277,#2278));
#658=EDGE_LOOP('',(#2279,#2280,#2281,#2282));
#659=EDGE_LOOP('',(#2283,#2284,#2285,#2286));
#660=EDGE_LOOP('',(#2287,#2288,#2289,#2290));
#661=EDGE_LOOP('',(#2291,#2292,#2293,#2294));
#662=EDGE_LOOP('',(#2295,#2296,#2297,#2298));
#663=EDGE_LOOP('',(#2299));
#664=EDGE_LOOP('',(#2300,#2301,#2302,#2303,#2304,#2305));
#665=EDGE_LOOP('',(#2306));
#666=EDGE_LOOP('',(#2307,#2308,#2309,#2310,#2311,#2312,#2313,#2314,#2315));
#667=EDGE_LOOP('',(#2316,#2317,#2318,#2319,#2320,#2321,#2322,#2323,#2324));
#668=EDGE_LOOP('',(#2325,#2326,#2327,#2328));
#669=EDGE_LOOP('',(#2329,#2330,#2331,#2332));
#670=EDGE_LOOP('',(#2333,#2334,#2335,#2336));
#671=EDGE_LOOP('',(#2337,#2338,#2339,#2340));
#672=EDGE_LOOP('',(#2341,#2342,#2343,#2344));
#673=EDGE_LOOP('',(#2345,#2346,#2347,#2348));
#674=EDGE_LOOP('',(#2349,#2350,#2351,#2352));
#675=EDGE_LOOP('',(#2353));
#676=EDGE_LOOP('',(#2354));
#677=EDGE_LOOP('',(#2355));
#678=EDGE_LOOP('',(#2356));
#679=EDGE_LOOP('',(#2357,#2358,#2359,#2360));
#680=EDGE_LOOP('',(#2361));
#681=EDGE_LOOP('',(#2362));
#682=EDGE_LOOP('',(#2363,#2364,#2365,#2366,#2367,#2368));
#683=EDGE_LOOP('',(#2369));
#684=EDGE_LOOP('',(#2370,#2371,#2372,#2373));
#685=EDGE_LOOP('',(#2374,#2375,#2376,#2377));
#686=EDGE_LOOP('',(#2378));
#687=EDGE_LOOP('',(#2379));
#688=EDGE_LOOP('',(#2380,#2381,#2382,#2383,#2384,#2385,#2386,#2387,#2388));
#689=EDGE_LOOP('',(#2389));
#690=EDGE_LOOP('',(#2390,#2391,#2392,#2393));
#691=EDGE_LOOP('',(#2394));
#692=EDGE_LOOP('',(#2395,#2396,#2397,#2398));
#693=EDGE_LOOP('',(#2399,#2400,#2401,#2402));
#694=EDGE_LOOP('',(#2403));
#695=EDGE_LOOP('',(#2404));
#696=EDGE_LOOP('',(#2405));
#697=EDGE_LOOP('',(#2406));
#698=EDGE_LOOP('',(#2407,#2408,#2409,#2410));
#699=EDGE_LOOP('',(#2411,#2412,#2413,#2414));
#700=EDGE_LOOP('',(#2415));
#701=EDGE_LOOP('',(#2416));
#702=EDGE_LOOP('',(#2417));
#703=EDGE_LOOP('',(#2418));
#704=EDGE_LOOP('',(#2419,#2420,#2421,#2422));
#705=EDGE_LOOP('',(#2423,#2424));
#706=EDGE_LOOP('',(#2425,#2426));
#707=EDGE_LOOP('',(#2427,#2428,#2429,#2430));
#708=EDGE_LOOP('',(#2431,#2432,#2433,#2434,#2435,#2436,#2437,#2438,#2439));
#709=EDGE_LOOP('',(#2440,#2441,#2442));
#710=CIRCLE('',#2791,0.3);
#711=CIRCLE('',#2792,0.3);
#712=CIRCLE('',#2793,0.3);
#713=CIRCLE('',#2794,0.3);
#714=CIRCLE('',#2803,0.275);
#715=CIRCLE('',#2804,0.275);
#716=CIRCLE('',#2806,0.275);
#717=CIRCLE('',#2808,0.275);
#718=CIRCLE('',#2810,0.51);
#719=CIRCLE('',#2811,0.51);
#720=CIRCLE('',#2818,0.31);
#721=CIRCLE('',#2819,0.31);
#722=CIRCLE('',#2821,0.31);
#723=CIRCLE('',#2822,0.31);
#724=CIRCLE('',#2840,0.275);
#725=CIRCLE('',#2841,0.275);
#726=CIRCLE('',#2843,0.31);
#727=CIRCLE('',#2844,0.31);
#728=CIRCLE('',#2846,0.7);
#729=CIRCLE('',#2847,0.7);
#730=CIRCLE('',#2849,0.6);
#731=CIRCLE('',#2852,0.6);
#732=CIRCLE('',#2855,0.31);
#733=CIRCLE('',#2856,0.31);
#734=CIRCLE('',#2858,0.31);
#735=CIRCLE('',#2859,0.31);
#736=CIRCLE('',#2865,0.6);
#737=CIRCLE('',#2868,0.6);
#738=CIRCLE('',#2871,0.6);
#739=CIRCLE('',#2872,0.6);
#740=CIRCLE('',#2883,0.21);
#741=CIRCLE('',#2884,0.21);
#742=CIRCLE('',#2887,0.7);
#743=CIRCLE('',#2888,0.7);
#744=CIRCLE('',#2901,0.24505);
#745=CIRCLE('',#2903,0.375);
#746=CIRCLE('',#2905,0.425);
#747=CIRCLE('',#2907,0.425);
#748=CIRCLE('',#2909,0.395);
#749=CIRCLE('',#2911,0.27);
#750=CIRCLE('',#2913,0.24505);
#751=CIRCLE('',#2918,0.31);
#752=CIRCLE('',#2919,0.31);
#753=CIRCLE('',#2921,0.31);
#754=CIRCLE('',#2922,0.31);
#755=CIRCLE('',#2924,0.6);
#756=CIRCLE('',#2925,0.6);
#757=CIRCLE('',#2928,0.6);
#758=CIRCLE('',#2931,0.6);
#759=CIRCLE('',#2937,0.34);
#760=CIRCLE('',#2938,0.34);
#761=CIRCLE('',#2941,0.31);
#762=CIRCLE('',#2942,0.31);
#763=CIRCLE('',#2944,0.31);
#764=CIRCLE('',#2945,0.31);
#765=CIRCLE('',#2952,0.5);
#766=CIRCLE('',#2958,0.5);
#767=CIRCLE('',#2962,0.3933);
#768=CIRCLE('',#2963,0.3933);
#769=CIRCLE('',#2965,0.32);
#770=CIRCLE('',#2968,0.6175);
#771=CIRCLE('',#2979,0.6175);
#772=CIRCLE('',#2981,0.6175);
#773=CIRCLE('',#2986,0.338975);
#774=CIRCLE('',#2987,0.338975);
#775=CIRCLE('',#2995,1.);
#776=CIRCLE('',#2996,1.);
#777=CIRCLE('',#3002,0.45);
#778=CIRCLE('',#3004,0.5);
#779=CIRCLE('',#3006,0.5);
#780=CIRCLE('',#3008,0.3);
#781=CIRCLE('',#3010,0.3);
#782=CIRCLE('',#3012,0.21);
#783=CIRCLE('',#3016,0.32);
#784=CIRCLE('',#3017,0.32);
#785=CIRCLE('',#3019,0.6);
#786=CIRCLE('',#3020,0.6);
#787=CIRCLE('',#3025,0.31);
#788=CIRCLE('',#3026,0.31);
#789=CIRCLE('',#3028,0.5);
#790=CIRCLE('',#3029,0.5);
#791=CIRCLE('',#3034,0.08);
#792=CIRCLE('',#3035,0.04);
#793=CIRCLE('',#3037,0.08);
#794=CIRCLE('',#3040,0.08);
#795=CIRCLE('',#3041,0.08);
#796=LINE('',#3862,#1016);
#797=LINE('',#3866,#1017);
#798=LINE('',#3870,#1018);
#799=LINE('',#3876,#1019);
#800=LINE('',#3878,#1020);
#801=LINE('',#3880,#1021);
#802=LINE('',#3882,#1022);
#803=LINE('',#3884,#1023);
#804=LINE('',#3886,#1024);
#805=LINE('',#3888,#1025);
#806=LINE('',#3890,#1026);
#807=LINE('',#3891,#1027);
#808=LINE('',#3894,#1028);
#809=LINE('',#3895,#1029);
#810=LINE('',#3898,#1030);
#811=LINE('',#3899,#1031);
#812=LINE('',#3902,#1032);
#813=LINE('',#3903,#1033);
#814=LINE('',#3906,#1034);
#815=LINE('',#3907,#1035);
#816=LINE('',#3909,#1036);
#817=LINE('',#3912,#1037);
#818=LINE('',#3914,#1038);
#819=LINE('',#3915,#1039);
#820=LINE('',#3918,#1040);
#821=LINE('',#3920,#1041);
#822=LINE('',#3922,#1042);
#823=LINE('',#3923,#1043);
#824=LINE('',#3926,#1044);
#825=LINE('',#3928,#1045);
#826=LINE('',#3930,#1046);
#827=LINE('',#3931,#1047);
#828=LINE('',#3934,#1048);
#829=LINE('',#3936,#1049);
#830=LINE('',#3938,#1050);
#831=LINE('',#3939,#1051);
#832=LINE('',#3947,#1052);
#833=LINE('',#3951,#1053);
#834=LINE('',#3956,#1054);
#835=LINE('',#3960,#1055);
#836=LINE('',#3962,#1056);
#837=LINE('',#3963,#1057);
#838=LINE('',#3966,#1058);
#839=LINE('',#3967,#1059);
#840=LINE('',#3970,#1060);
#841=LINE('',#3971,#1061);
#842=LINE('',#3973,#1062);
#843=LINE('',#3979,#1063);
#844=LINE('',#3985,#1064);
#845=LINE('',#3989,#1065);
#846=LINE('',#3991,#1066);
#847=LINE('',#3992,#1067);
#848=LINE('',#3995,#1068);
#849=LINE('',#3996,#1069);
#850=LINE('',#3999,#1070);
#851=LINE('',#4000,#1071);
#852=LINE('',#4002,#1072);
#853=LINE('',#4006,#1073);
#854=LINE('',#4008,#1074);
#855=LINE('',#4009,#1075);
#856=LINE('',#4012,#1076);
#857=LINE('',#4013,#1077);
#858=LINE('',#4016,#1078);
#859=LINE('',#4017,#1079);
#860=LINE('',#4019,#1080);
#861=LINE('',#4023,#1081);
#862=LINE('',#4024,#1082);
#863=LINE('',#4027,#1083);
#864=LINE('',#4028,#1084);
#865=LINE('',#4030,#1085);
#866=LINE('',#4038,#1086);
#867=LINE('',#4044,#1087);
#868=LINE('',#4049,#1088);
#869=LINE('',#4053,#1089);
#870=LINE('',#4057,#1090);
#871=LINE('',#4060,#1091);
#872=LINE('',#4063,#1092);
#873=LINE('',#4064,#1093);
#874=LINE('',#4067,#1094);
#875=LINE('',#4070,#1095);
#876=LINE('',#4075,#1096);
#877=LINE('',#4081,#1097);
#878=LINE('',#4086,#1098);
#879=LINE('',#4088,#1099);
#880=LINE('',#4090,#1100);
#881=LINE('',#4091,#1101);
#882=LINE('',#4095,#1102);
#883=LINE('',#4097,#1103);
#884=LINE('',#4099,#1104);
#885=LINE('',#4100,#1105);
#886=LINE('',#4104,#1106);
#887=LINE('',#4105,#1107);
#888=LINE('',#4106,#1108);
#889=LINE('',#4108,#1109);
#890=LINE('',#4109,#1110);
#891=LINE('',#4113,#1111);
#892=LINE('',#4115,#1112);
#893=LINE('',#4118,#1113);
#894=LINE('',#4121,#1114);
#895=LINE('',#4123,#1115);
#896=LINE('',#4124,#1116);
#897=LINE('',#4127,#1117);
#898=LINE('',#4129,#1118);
#899=LINE('',#4132,#1119);
#900=LINE('',#4133,#1120);
#901=LINE('',#4138,#1121);
#902=LINE('',#4144,#1122);
#903=LINE('',#4146,#1123);
#904=LINE('',#4148,#1124);
#905=LINE('',#4149,#1125);
#906=LINE('',#4152,#1126);
#907=LINE('',#4153,#1127);
#908=LINE('',#4156,#1128);
#909=LINE('',#4157,#1129);
#910=LINE('',#4160,#1130);
#911=LINE('',#4161,#1131);
#912=LINE('',#4163,#1132);
#913=LINE('',#4170,#1133);
#914=LINE('',#4177,#1134);
#915=LINE('',#4185,#1135);
#916=LINE('',#4187,#1136);
#917=LINE('',#4189,#1137);
#918=LINE('',#4190,#1138);
#919=LINE('',#4193,#1139);
#920=LINE('',#4195,#1140);
#921=LINE('',#4196,#1141);
#922=LINE('',#4199,#1142);
#923=LINE('',#4201,#1143);
#924=LINE('',#4202,#1144);
#925=LINE('',#4205,#1145);
#926=LINE('',#4207,#1146);
#927=LINE('',#4208,#1147);
#928=LINE('',#4211,#1148);
#929=LINE('',#4213,#1149);
#930=LINE('',#4214,#1150);
#931=LINE('',#4216,#1151);
#932=LINE('',#4217,#1152);
#933=LINE('',#4229,#1153);
#934=LINE('',#4233,#1154);
#935=LINE('',#4237,#1155);
#936=LINE('',#4244,#1156);
#937=LINE('',#4246,#1157);
#938=LINE('',#4253,#1158);
#939=LINE('',#4259,#1159);
#940=LINE('',#4264,#1160);
#941=LINE('',#4268,#1161);
#942=LINE('',#4272,#1162);
#943=LINE('',#4274,#1163);
#944=LINE('',#4275,#1164);
#945=LINE('',#4278,#1165);
#946=LINE('',#4282,#1166);
#947=LINE('',#4283,#1167);
#948=LINE('',#4294,#1168);
#949=LINE('',#4301,#1169);
#950=LINE('',#4307,#1170);
#951=LINE('',#4312,#1171);
#952=LINE('',#4314,#1172);
#953=LINE('',#4316,#1173);
#954=LINE('',#4317,#1174);
#955=LINE('',#4321,#1175);
#956=LINE('',#4323,#1176);
#957=LINE('',#4325,#1177);
#958=LINE('',#4326,#1178);
#959=LINE('',#4329,#1179);
#960=LINE('',#4330,#1180);
#961=LINE('',#4332,#1181);
#962=LINE('',#4334,#1182);
#963=LINE('',#4336,#1183);
#964=LINE('',#4337,#1184);
#965=LINE('',#4341,#1185);
#966=LINE('',#4342,#1186);
#967=LINE('',#4343,#1187);
#968=LINE('',#4346,#1188);
#969=LINE('',#4347,#1189);
#970=LINE('',#4349,#1190);
#971=LINE('',#4353,#1191);
#972=LINE('',#4355,#1192);
#973=LINE('',#4356,#1193);
#974=LINE('',#4359,#1194);
#975=LINE('',#4364,#1195);
#976=LINE('',#4371,#1196);
#977=LINE('',#4376,#1197);
#978=LINE('',#4382,#1198);
#979=LINE('',#4408,#1199);
#980=LINE('',#4410,#1200);
#981=LINE('',#4411,#1201);
#982=LINE('',#4414,#1202);
#983=LINE('',#4415,#1203);
#984=LINE('',#4418,#1204);
#985=LINE('',#4419,#1205);
#986=LINE('',#4422,#1206);
#987=LINE('',#4423,#1207);
#988=LINE('',#4426,#1208);
#989=LINE('',#4427,#1209);
#990=LINE('',#4429,#1210);
#991=LINE('',#4444,#1211);
#992=LINE('',#4465,#1212);
#993=LINE('',#4490,#1213);
#994=LINE('',#4491,#1214);
#995=LINE('',#4493,#1215);
#996=LINE('',#4495,#1216);
#997=LINE('',#4500,#1217);
#998=LINE('',#4503,#1218);
#999=LINE('',#4505,#1219);
#1000=LINE('',#4514,#1220);
#1001=LINE('',#4533,#1221);
#1002=LINE('',#4603,#1222);
#1003=LINE('',#4607,#1223);
#1004=LINE('',#4614,#1224);
#1005=LINE('',#4615,#1225);
#1006=LINE('',#4619,#1226);
#1007=LINE('',#4626,#1227);
#1008=LINE('',#4632,#1228);
#1009=LINE('',#4641,#1229);
#1010=LINE('',#4647,#1230);
#1011=LINE('',#4714,#1231);
#1012=LINE('',#4717,#1232);
#1013=LINE('',#4719,#1233);
#1014=LINE('',#4720,#1234);
#1015=LINE('',#4724,#1235);
#1016=VECTOR('',#3078,1.);
#1017=VECTOR('',#3081,1.);
#1018=VECTOR('',#3084,0.3);
#1019=VECTOR('',#3093,1.);
#1020=VECTOR('',#3094,1.);
#1021=VECTOR('',#3095,1.);
#1022=VECTOR('',#3096,1.);
#1023=VECTOR('',#3097,1.);
#1024=VECTOR('',#3098,1.);
#1025=VECTOR('',#3099,1.);
#1026=VECTOR('',#3100,1.);
#1027=VECTOR('',#3101,1.);
#1028=VECTOR('',#3104,1.);
#1029=VECTOR('',#3105,1.);
#1030=VECTOR('',#3108,1.);
#1031=VECTOR('',#3109,1.);
#1032=VECTOR('',#3112,1.);
#1033=VECTOR('',#3113,1.);
#1034=VECTOR('',#3116,1.);
#1035=VECTOR('',#3117,1.);
#1036=VECTOR('',#3120,1.);
#1037=VECTOR('',#3123,1.);
#1038=VECTOR('',#3124,1.);
#1039=VECTOR('',#3125,1.);
#1040=VECTOR('',#3126,1.);
#1041=VECTOR('',#3127,1.);
#1042=VECTOR('',#3128,1.);
#1043=VECTOR('',#3129,1.);
#1044=VECTOR('',#3130,1.);
#1045=VECTOR('',#3131,1.);
#1046=VECTOR('',#3132,1.);
#1047=VECTOR('',#3133,1.);
#1048=VECTOR('',#3134,1.);
#1049=VECTOR('',#3135,1.);
#1050=VECTOR('',#3136,1.);
#1051=VECTOR('',#3137,1.);
#1052=VECTOR('',#3146,0.275);
#1053=VECTOR('',#3151,0.275);
#1054=VECTOR('',#3156,0.51);
#1055=VECTOR('',#3161,1.);
#1056=VECTOR('',#3162,1.);
#1057=VECTOR('',#3163,1.);
#1058=VECTOR('',#3166,1.);
#1059=VECTOR('',#3167,1.);
#1060=VECTOR('',#3170,1.);
#1061=VECTOR('',#3171,1.);
#1062=VECTOR('',#3174,1.);
#1063=VECTOR('',#3181,0.31);
#1064=VECTOR('',#3188,0.31);
#1065=VECTOR('',#3193,1.);
#1066=VECTOR('',#3194,1.);
#1067=VECTOR('',#3195,1.);
#1068=VECTOR('',#3198,1.);
#1069=VECTOR('',#3199,1.);
#1070=VECTOR('',#3202,1.);
#1071=VECTOR('',#3203,1.);
#1072=VECTOR('',#3206,1.);
#1073=VECTOR('',#3211,1.);
#1074=VECTOR('',#3212,1.);
#1075=VECTOR('',#3213,1.);
#1076=VECTOR('',#3216,1.);
#1077=VECTOR('',#3217,1.);
#1078=VECTOR('',#3220,1.);
#1079=VECTOR('',#3221,1.);
#1080=VECTOR('',#3224,1.);
#1081=VECTOR('',#3229,1.);
#1082=VECTOR('',#3230,1.);
#1083=VECTOR('',#3233,1.);
#1084=VECTOR('',#3234,1.);
#1085=VECTOR('',#3237,1.);
#1086=VECTOR('',#3248,0.275);
#1087=VECTOR('',#3255,0.31);
#1088=VECTOR('',#3260,1.);
#1089=VECTOR('',#3263,1.);
#1090=VECTOR('',#3268,1.);
#1091=VECTOR('',#3271,1.);
#1092=VECTOR('',#3274,1.);
#1093=VECTOR('',#3275,1.);
#1094=VECTOR('',#3278,1.);
#1095=VECTOR('',#3283,1.);
#1096=VECTOR('',#3288,0.31);
#1097=VECTOR('',#3295,0.31);
#1098=VECTOR('',#3300,1.);
#1099=VECTOR('',#3301,1.);
#1100=VECTOR('',#3302,1.);
#1101=VECTOR('',#3303,1.);
#1102=VECTOR('',#3306,1.);
#1103=VECTOR('',#3307,1.);
#1104=VECTOR('',#3308,1.);
#1105=VECTOR('',#3309,1.);
#1106=VECTOR('',#3312,1.);
#1107=VECTOR('',#3313,1.);
#1108=VECTOR('',#3314,1.);
#1109=VECTOR('',#3317,1.);
#1110=VECTOR('',#3318,1.);
#1111=VECTOR('',#3321,1.);
#1112=VECTOR('',#3322,1.);
#1113=VECTOR('',#3325,1.);
#1114=VECTOR('',#3328,1.);
#1115=VECTOR('',#3329,1.);
#1116=VECTOR('',#3330,1.);
#1117=VECTOR('',#3333,1.);
#1118=VECTOR('',#3334,1.);
#1119=VECTOR('',#3339,1.);
#1120=VECTOR('',#3340,1.);
#1121=VECTOR('',#3345,0.6);
#1122=VECTOR('',#3354,1.);
#1123=VECTOR('',#3355,1.);
#1124=VECTOR('',#3356,1.);
#1125=VECTOR('',#3357,1.);
#1126=VECTOR('',#3360,1.);
#1127=VECTOR('',#3361,1.);
#1128=VECTOR('',#3364,1.);
#1129=VECTOR('',#3365,1.);
#1130=VECTOR('',#3368,1.);
#1131=VECTOR('',#3369,1.);
#1132=VECTOR('',#3372,1.);
#1133=VECTOR('',#3381,0.21);
#1134=VECTOR('',#3390,0.7);
#1135=VECTOR('',#3401,1.);
#1136=VECTOR('',#3402,1.);
#1137=VECTOR('',#3403,1.);
#1138=VECTOR('',#3404,1.);
#1139=VECTOR('',#3407,1.);
#1140=VECTOR('',#3408,1.);
#1141=VECTOR('',#3409,1.);
#1142=VECTOR('',#3412,1.);
#1143=VECTOR('',#3413,1.);
#1144=VECTOR('',#3414,1.);
#1145=VECTOR('',#3417,1.);
#1146=VECTOR('',#3418,1.);
#1147=VECTOR('',#3419,1.);
#1148=VECTOR('',#3422,1.);
#1149=VECTOR('',#3423,1.);
#1150=VECTOR('',#3424,1.);
#1151=VECTOR('',#3427,1.);
#1152=VECTOR('',#3428,1.);
#1153=VECTOR('',#3445,0.4);
#1154=VECTOR('',#3450,0.425);
#1155=VECTOR('',#3455,0.41);
#1156=VECTOR('',#3464,0.26);
#1157=VECTOR('',#3467,0.25);
#1158=VECTOR('',#3476,0.31);
#1159=VECTOR('',#3483,0.31);
#1160=VECTOR('',#3488,1.);
#1161=VECTOR('',#3491,1.);
#1162=VECTOR('',#3496,1.);
#1163=VECTOR('',#3497,1.);
#1164=VECTOR('',#3498,1.);
#1165=VECTOR('',#3501,1.);
#1166=VECTOR('',#3506,1.);
#1167=VECTOR('',#3507,1.);
#1168=VECTOR('',#3524,0.34);
#1169=VECTOR('',#3533,0.31);
#1170=VECTOR('',#3540,0.31);
#1171=VECTOR('',#3545,1.);
#1172=VECTOR('',#3546,1.);
#1173=VECTOR('',#3547,1.);
#1174=VECTOR('',#3548,1.);
#1175=VECTOR('',#3551,1.);
#1176=VECTOR('',#3552,1.);
#1177=VECTOR('',#3553,1.);
#1178=VECTOR('',#3554,1.);
#1179=VECTOR('',#3557,1.);
#1180=VECTOR('',#3558,1.);
#1181=VECTOR('',#3559,1.);
#1182=VECTOR('',#3560,1.);
#1183=VECTOR('',#3561,1.);
#1184=VECTOR('',#3562,1.);
#1185=VECTOR('',#3565,1.);
#1186=VECTOR('',#3566,1.);
#1187=VECTOR('',#3567,1.);
#1188=VECTOR('',#3570,1.);
#1189=VECTOR('',#3571,1.);
#1190=VECTOR('',#3574,1.);
#1191=VECTOR('',#3579,1.);
#1192=VECTOR('',#3580,1.);
#1193=VECTOR('',#3581,1.);
#1194=VECTOR('',#3586,1.);
#1195=VECTOR('',#3593,0.5);
#1196=VECTOR('',#3602,0.4);
#1197=VECTOR('',#3609,0.36);
#1198=VECTOR('',#3616,0.734027674973257);
#1199=VECTOR('',#3619,1.);
#1200=VECTOR('',#3620,1.);
#1201=VECTOR('',#3621,1.);
#1202=VECTOR('',#3624,1.);
#1203=VECTOR('',#3625,1.);
#1204=VECTOR('',#3628,1.);
#1205=VECTOR('',#3629,1.);
#1206=VECTOR('',#3632,1.);
#1207=VECTOR('',#3633,1.);
#1208=VECTOR('',#3636,1.);
#1209=VECTOR('',#3637,1.);
#1210=VECTOR('',#3640,1.);
#1211=VECTOR('',#3649,0.734027674973257);
#1212=VECTOR('',#3656,0.734027674973257);
#1213=VECTOR('',#3659,1.);
#1214=VECTOR('',#3660,1.);
#1215=VECTOR('',#3663,1.);
#1216=VECTOR('',#3666,1.);
#1217=VECTOR('',#3671,0.4);
#1218=VECTOR('',#3676,1.);
#1219=VECTOR('',#3679,1.);
#1220=VECTOR('',#3692,1.);
#1221=VECTOR('',#3703,0.08);
#1222=VECTOR('',#3712,0.475);
#1223=VECTOR('',#3717,0.5);
#1224=VECTOR('',#3726,0.3);
#1225=VECTOR('',#3727,0.3);
#1226=VECTOR('',#3732,0.255);
#1227=VECTOR('',#3741,0.32);
#1228=VECTOR('',#3748,0.6);
#1229=VECTOR('',#3761,0.31);
#1230=VECTOR('',#3768,0.5);
#1231=VECTOR('',#3787,1.);
#1232=VECTOR('',#3790,1.);
#1233=VECTOR('',#3791,1.);
#1234=VECTOR('',#3792,1.);
#1235=VECTOR('',#3797,0.08);
#1236=VERTEX_POINT('',#3860);
#1237=VERTEX_POINT('',#3861);
#1238=VERTEX_POINT('',#3863);
#1239=VERTEX_POINT('',#3865);
#1240=VERTEX_POINT('',#3867);
#1241=VERTEX_POINT('',#3869);
#1242=VERTEX_POINT('',#3875);
#1243=VERTEX_POINT('',#3877);
#1244=VERTEX_POINT('',#3879);
#1245=VERTEX_POINT('',#3881);
#1246=VERTEX_POINT('',#3883);
#1247=VERTEX_POINT('',#3885);
#1248=VERTEX_POINT('',#3887);
#1249=VERTEX_POINT('',#3889);
#1250=VERTEX_POINT('',#3893);
#1251=VERTEX_POINT('',#3897);
#1252=VERTEX_POINT('',#3901);
#1253=VERTEX_POINT('',#3905);
#1254=VERTEX_POINT('',#3911);
#1255=VERTEX_POINT('',#3913);
#1256=VERTEX_POINT('',#3916);
#1257=VERTEX_POINT('',#3917);
#1258=VERTEX_POINT('',#3919);
#1259=VERTEX_POINT('',#3921);
#1260=VERTEX_POINT('',#3924);
#1261=VERTEX_POINT('',#3925);
#1262=VERTEX_POINT('',#3927);
#1263=VERTEX_POINT('',#3929);
#1264=VERTEX_POINT('',#3932);
#1265=VERTEX_POINT('',#3933);
#1266=VERTEX_POINT('',#3935);
#1267=VERTEX_POINT('',#3937);
#1268=VERTEX_POINT('',#3940);
#1269=VERTEX_POINT('',#3942);
#1270=VERTEX_POINT('',#3945);
#1271=VERTEX_POINT('',#3949);
#1272=VERTEX_POINT('',#3953);
#1273=VERTEX_POINT('',#3955);
#1274=VERTEX_POINT('',#3959);
#1275=VERTEX_POINT('',#3961);
#1276=VERTEX_POINT('',#3965);
#1277=VERTEX_POINT('',#3969);
#1278=VERTEX_POINT('',#3976);
#1279=VERTEX_POINT('',#3978);
#1280=VERTEX_POINT('',#3982);
#1281=VERTEX_POINT('',#3984);
#1282=VERTEX_POINT('',#3988);
#1283=VERTEX_POINT('',#3990);
#1284=VERTEX_POINT('',#3994);
#1285=VERTEX_POINT('',#3998);
#1286=VERTEX_POINT('',#4005);
#1287=VERTEX_POINT('',#4007);
#1288=VERTEX_POINT('',#4011);
#1289=VERTEX_POINT('',#4015);
#1290=VERTEX_POINT('',#4022);
#1291=VERTEX_POINT('',#4026);
#1292=VERTEX_POINT('',#4035);
#1293=VERTEX_POINT('',#4037);
#1294=VERTEX_POINT('',#4041);
#1295=VERTEX_POINT('',#4043);
#1296=VERTEX_POINT('',#4047);
#1297=VERTEX_POINT('',#4048);
#1298=VERTEX_POINT('',#4050);
#1299=VERTEX_POINT('',#4052);
#1300=VERTEX_POINT('',#4056);
#1301=VERTEX_POINT('',#4058);
#1302=VERTEX_POINT('',#4062);
#1303=VERTEX_POINT('',#4066);
#1304=VERTEX_POINT('',#4072);
#1305=VERTEX_POINT('',#4074);
#1306=VERTEX_POINT('',#4078);
#1307=VERTEX_POINT('',#4080);
#1308=VERTEX_POINT('',#4084);
#1309=VERTEX_POINT('',#4085);
#1310=VERTEX_POINT('',#4087);
#1311=VERTEX_POINT('',#4089);
#1312=VERTEX_POINT('',#4093);
#1313=VERTEX_POINT('',#4094);
#1314=VERTEX_POINT('',#4096);
#1315=VERTEX_POINT('',#4098);
#1316=VERTEX_POINT('',#4102);
#1317=VERTEX_POINT('',#4103);
#1318=VERTEX_POINT('',#4111);
#1319=VERTEX_POINT('',#4112);
#1320=VERTEX_POINT('',#4114);
#1321=VERTEX_POINT('',#4116);
#1322=VERTEX_POINT('',#4120);
#1323=VERTEX_POINT('',#4122);
#1324=VERTEX_POINT('',#4126);
#1325=VERTEX_POINT('',#4128);
#1326=VERTEX_POINT('',#4135);
#1327=VERTEX_POINT('',#4137);
#1328=VERTEX_POINT('',#4143);
#1329=VERTEX_POINT('',#4145);
#1330=VERTEX_POINT('',#4147);
#1331=VERTEX_POINT('',#4151);
#1332=VERTEX_POINT('',#4155);
#1333=VERTEX_POINT('',#4159);
#1334=VERTEX_POINT('',#4167);
#1335=VERTEX_POINT('',#4169);
#1336=VERTEX_POINT('',#4174);
#1337=VERTEX_POINT('',#4176);
#1338=VERTEX_POINT('',#4183);
#1339=VERTEX_POINT('',#4184);
#1340=VERTEX_POINT('',#4186);
#1341=VERTEX_POINT('',#4188);
#1342=VERTEX_POINT('',#4192);
#1343=VERTEX_POINT('',#4194);
#1344=VERTEX_POINT('',#4198);
#1345=VERTEX_POINT('',#4200);
#1346=VERTEX_POINT('',#4204);
#1347=VERTEX_POINT('',#4206);
#1348=VERTEX_POINT('',#4210);
#1349=VERTEX_POINT('',#4212);
#1350=VERTEX_POINT('',#4221);
#1351=VERTEX_POINT('',#4224);
#1352=VERTEX_POINT('',#4227);
#1353=VERTEX_POINT('',#4231);
#1354=VERTEX_POINT('',#4235);
#1355=VERTEX_POINT('',#4239);
#1356=VERTEX_POINT('',#4242);
#1357=VERTEX_POINT('',#4250);
#1358=VERTEX_POINT('',#4252);
#1359=VERTEX_POINT('',#4256);
#1360=VERTEX_POINT('',#4258);
#1361=VERTEX_POINT('',#4262);
#1362=VERTEX_POINT('',#4263);
#1363=VERTEX_POINT('',#4265);
#1364=VERTEX_POINT('',#4267);
#1365=VERTEX_POINT('',#4271);
#1366=VERTEX_POINT('',#4273);
#1367=VERTEX_POINT('',#4277);
#1368=VERTEX_POINT('',#4281);
#1369=VERTEX_POINT('',#4291);
#1370=VERTEX_POINT('',#4293);
#1371=VERTEX_POINT('',#4298);
#1372=VERTEX_POINT('',#4300);
#1373=VERTEX_POINT('',#4304);
#1374=VERTEX_POINT('',#4306);
#1375=VERTEX_POINT('',#4310);
#1376=VERTEX_POINT('',#4311);
#1377=VERTEX_POINT('',#4313);
#1378=VERTEX_POINT('',#4315);
#1379=VERTEX_POINT('',#4319);
#1380=VERTEX_POINT('',#4320);
#1381=VERTEX_POINT('',#4322);
#1382=VERTEX_POINT('',#4324);
#1383=VERTEX_POINT('',#4328);
#1384=VERTEX_POINT('',#4331);
#1385=VERTEX_POINT('',#4333);
#1386=VERTEX_POINT('',#4335);
#1387=VERTEX_POINT('',#4339);
#1388=VERTEX_POINT('',#4340);
#1389=VERTEX_POINT('',#4345);
#1390=VERTEX_POINT('',#4350);
#1391=VERTEX_POINT('',#4354);
#1392=VERTEX_POINT('',#4362);
#1393=VERTEX_POINT('',#4368);
#1394=VERTEX_POINT('',#4370);
#1395=VERTEX_POINT('',#4374);
#1396=VERTEX_POINT('',#4379);
#1397=VERTEX_POINT('',#4381);
#1398=VERTEX_POINT('',#4383);
#1399=VERTEX_POINT('',#4387);
#1400=VERTEX_POINT('',#4391);
#1401=VERTEX_POINT('',#4395);
#1402=VERTEX_POINT('',#4399);
#1403=VERTEX_POINT('',#4407);
#1404=VERTEX_POINT('',#4409);
#1405=VERTEX_POINT('',#4413);
#1406=VERTEX_POINT('',#4417);
#1407=VERTEX_POINT('',#4421);
#1408=VERTEX_POINT('',#4425);
#1409=VERTEX_POINT('',#4434);
#1410=VERTEX_POINT('',#4435);
#1411=VERTEX_POINT('',#4439);
#1412=VERTEX_POINT('',#4443);
#1413=VERTEX_POINT('',#4446);
#1414=VERTEX_POINT('',#4450);
#1415=VERTEX_POINT('',#4454);
#1416=VERTEX_POINT('',#4462);
#1417=VERTEX_POINT('',#4464);
#1418=VERTEX_POINT('',#4466);
#1419=VERTEX_POINT('',#4470);
#1420=VERTEX_POINT('',#4474);
#1421=VERTEX_POINT('',#4478);
#1422=VERTEX_POINT('',#4482);
#1423=VERTEX_POINT('',#4497);
#1424=VERTEX_POINT('',#4499);
#1425=VERTEX_POINT('',#4511);
#1426=VERTEX_POINT('',#4513);
#1427=VERTEX_POINT('',#4520);
#1428=VERTEX_POINT('',#4521);
#1429=VERTEX_POINT('',#4532);
#1430=VERTEX_POINT('',#4568);
#1431=VERTEX_POINT('',#4598);
#1432=VERTEX_POINT('',#4601);
#1433=VERTEX_POINT('',#4605);
#1434=VERTEX_POINT('',#4609);
#1435=VERTEX_POINT('',#4612);
#1436=VERTEX_POINT('',#4617);
#1437=VERTEX_POINT('',#4623);
#1438=VERTEX_POINT('',#4625);
#1439=VERTEX_POINT('',#4629);
#1440=VERTEX_POINT('',#4631);
#1441=VERTEX_POINT('',#4638);
#1442=VERTEX_POINT('',#4640);
#1443=VERTEX_POINT('',#4644);
#1444=VERTEX_POINT('',#4646);
#1445=VERTEX_POINT('',#4653);
#1446=VERTEX_POINT('',#4656);
#1447=VERTEX_POINT('',#4657);
#1448=VERTEX_POINT('',#4711);
#1449=VERTEX_POINT('',#4712);
#1450=VERTEX_POINT('',#4716);
#1451=VERTEX_POINT('',#4718);
#1452=VERTEX_POINT('',#4722);
#1453=EDGE_CURVE('',#1236,#1237,#796,.T.);
#1454=EDGE_CURVE('',#1238,#1236,#710,.T.);
#1455=EDGE_CURVE('',#1238,#1239,#797,.T.);
#1456=EDGE_CURVE('',#1240,#1239,#711,.T.);
#1457=EDGE_CURVE('',#1240,#1241,#798,.T.);
#1458=EDGE_CURVE('',#1241,#1241,#712,.T.);
#1459=EDGE_CURVE('',#1237,#1240,#713,.T.);
#1460=EDGE_CURVE('',#1239,#1242,#799,.T.);
#1461=EDGE_CURVE('',#1242,#1243,#800,.T.);
#1462=EDGE_CURVE('',#1244,#1243,#801,.T.);
#1463=EDGE_CURVE('',#1245,#1244,#802,.T.);
#1464=EDGE_CURVE('',#1245,#1246,#803,.T.);
#1465=EDGE_CURVE('',#1246,#1247,#804,.T.);
#1466=EDGE_CURVE('',#1248,#1247,#805,.T.);
#1467=EDGE_CURVE('',#1248,#1249,#806,.T.);
#1468=EDGE_CURVE('',#1249,#1237,#807,.T.);
#1469=EDGE_CURVE('',#1250,#1249,#808,.T.);
#1470=EDGE_CURVE('',#1236,#1250,#809,.T.);
#1471=EDGE_CURVE('',#1251,#1238,#810,.T.);
#1472=EDGE_CURVE('',#1251,#1242,#811,.T.);
#1473=EDGE_CURVE('',#1252,#1251,#812,.T.);
#1474=EDGE_CURVE('',#1243,#1252,#813,.T.);
#1475=EDGE_CURVE('',#1253,#1248,#814,.T.);
#1476=EDGE_CURVE('',#1250,#1253,#815,.T.);
#1477=EDGE_CURVE('',#1252,#1253,#816,.T.);
#1478=EDGE_CURVE('',#1247,#1254,#817,.T.);
#1479=EDGE_CURVE('',#1254,#1255,#818,.T.);
#1480=EDGE_CURVE('',#1255,#1244,#819,.T.);
#1481=EDGE_CURVE('',#1256,#1257,#820,.T.);
#1482=EDGE_CURVE('',#1257,#1258,#821,.T.);
#1483=EDGE_CURVE('',#1258,#1259,#822,.T.);
#1484=EDGE_CURVE('',#1259,#1256,#823,.T.);
#1485=EDGE_CURVE('',#1260,#1261,#824,.T.);
#1486=EDGE_CURVE('',#1261,#1262,#825,.T.);
#1487=EDGE_CURVE('',#1262,#1263,#826,.T.);
#1488=EDGE_CURVE('',#1263,#1260,#827,.T.);
#1489=EDGE_CURVE('',#1264,#1265,#828,.T.);
#1490=EDGE_CURVE('',#1265,#1266,#829,.T.);
#1491=EDGE_CURVE('',#1266,#1267,#830,.T.);
#1492=EDGE_CURVE('',#1267,#1264,#831,.T.);
#1493=EDGE_CURVE('',#1268,#1268,#714,.T.);
#1494=EDGE_CURVE('',#1269,#1269,#715,.T.);
#1495=EDGE_CURVE('',#1270,#1270,#716,.T.);
#1496=EDGE_CURVE('',#1270,#1269,#832,.T.);
#1497=EDGE_CURVE('',#1271,#1271,#717,.T.);
#1498=EDGE_CURVE('',#1271,#1268,#833,.T.);
#1499=EDGE_CURVE('',#1272,#1272,#718,.T.);
#1500=EDGE_CURVE('',#1272,#1273,#834,.T.);
#1501=EDGE_CURVE('',#1273,#1273,#719,.T.);
#1502=EDGE_CURVE('',#1265,#1274,#835,.T.);
#1503=EDGE_CURVE('',#1274,#1275,#836,.T.);
#1504=EDGE_CURVE('',#1275,#1266,#837,.T.);
#1505=EDGE_CURVE('',#1276,#1264,#838,.T.);
#1506=EDGE_CURVE('',#1274,#1276,#839,.T.);
#1507=EDGE_CURVE('',#1275,#1277,#840,.T.);
#1508=EDGE_CURVE('',#1267,#1277,#841,.T.);
#1509=EDGE_CURVE('',#1277,#1276,#842,.T.);
#1510=EDGE_CURVE('',#1278,#1278,#720,.T.);
#1511=EDGE_CURVE('',#1278,#1279,#843,.T.);
#1512=EDGE_CURVE('',#1279,#1279,#721,.T.);
#1513=EDGE_CURVE('',#1280,#1280,#722,.T.);
#1514=EDGE_CURVE('',#1280,#1281,#844,.T.);
#1515=EDGE_CURVE('',#1281,#1281,#723,.T.);
#1516=EDGE_CURVE('',#1261,#1282,#845,.T.);
#1517=EDGE_CURVE('',#1282,#1283,#846,.T.);
#1518=EDGE_CURVE('',#1283,#1262,#847,.T.);
#1519=EDGE_CURVE('',#1284,#1260,#848,.T.);
#1520=EDGE_CURVE('',#1282,#1284,#849,.T.);
#1521=EDGE_CURVE('',#1283,#1285,#850,.T.);
#1522=EDGE_CURVE('',#1263,#1285,#851,.T.);
#1523=EDGE_CURVE('',#1285,#1284,#852,.T.);
#1524=EDGE_CURVE('',#1257,#1286,#853,.T.);
#1525=EDGE_CURVE('',#1286,#1287,#854,.T.);
#1526=EDGE_CURVE('',#1287,#1258,#855,.T.);
#1527=EDGE_CURVE('',#1288,#1256,#856,.T.);
#1528=EDGE_CURVE('',#1286,#1288,#857,.T.);
#1529=EDGE_CURVE('',#1287,#1289,#858,.T.);
#1530=EDGE_CURVE('',#1259,#1289,#859,.T.);
#1531=EDGE_CURVE('',#1289,#1288,#860,.T.);
#1532=EDGE_CURVE('',#1290,#1245,#861,.T.);
#1533=EDGE_CURVE('',#1290,#1255,#862,.T.);
#1534=EDGE_CURVE('',#1291,#1290,#863,.T.);
#1535=EDGE_CURVE('',#1291,#1254,#864,.T.);
#1536=EDGE_CURVE('',#1246,#1291,#865,.T.);
#1537=EDGE_CURVE('',#1292,#1292,#724,.T.);
#1538=EDGE_CURVE('',#1292,#1293,#866,.T.);
#1539=EDGE_CURVE('',#1293,#1293,#725,.T.);
#1540=EDGE_CURVE('',#1294,#1294,#726,.T.);
#1541=EDGE_CURVE('',#1294,#1295,#867,.T.);
#1542=EDGE_CURVE('',#1295,#1295,#727,.T.);
#1543=EDGE_CURVE('',#1296,#1297,#868,.T.);
#1544=EDGE_CURVE('',#1298,#1296,#728,.T.);
#1545=EDGE_CURVE('',#1299,#1298,#869,.T.);
#1546=EDGE_CURVE('',#1299,#1297,#729,.T.);
#1547=EDGE_CURVE('',#1300,#1299,#870,.T.);
#1548=EDGE_CURVE('',#1301,#1300,#730,.T.);
#1549=EDGE_CURVE('',#1297,#1301,#871,.T.);
#1550=EDGE_CURVE('',#1302,#1298,#872,.T.);
#1551=EDGE_CURVE('',#1300,#1302,#873,.T.);
#1552=EDGE_CURVE('',#1296,#1303,#874,.T.);
#1553=EDGE_CURVE('',#1302,#1303,#731,.T.);
#1554=EDGE_CURVE('',#1303,#1301,#875,.T.);
#1555=EDGE_CURVE('',#1304,#1304,#732,.T.);
#1556=EDGE_CURVE('',#1304,#1305,#876,.T.);
#1557=EDGE_CURVE('',#1305,#1305,#733,.T.);
#1558=EDGE_CURVE('',#1306,#1306,#734,.T.);
#1559=EDGE_CURVE('',#1306,#1307,#877,.T.);
#1560=EDGE_CURVE('',#1307,#1307,#735,.T.);
#1561=EDGE_CURVE('',#1308,#1309,#878,.T.);
#1562=EDGE_CURVE('',#1308,#1310,#879,.T.);
#1563=EDGE_CURVE('',#1311,#1310,#880,.T.);
#1564=EDGE_CURVE('',#1309,#1311,#881,.T.);
#1565=EDGE_CURVE('',#1312,#1313,#882,.T.);
#1566=EDGE_CURVE('',#1313,#1314,#883,.T.);
#1567=EDGE_CURVE('',#1314,#1315,#884,.T.);
#1568=EDGE_CURVE('',#1315,#1312,#885,.T.);
#1569=EDGE_CURVE('',#1316,#1317,#886,.T.);
#1570=EDGE_CURVE('',#1316,#1314,#887,.T.);
#1571=EDGE_CURVE('',#1317,#1313,#888,.T.);
#1572=EDGE_CURVE('',#1310,#1316,#889,.T.);
#1573=EDGE_CURVE('',#1317,#1311,#890,.T.);
#1574=EDGE_CURVE('',#1318,#1319,#891,.T.);
#1575=EDGE_CURVE('',#1320,#1319,#892,.T.);
#1576=EDGE_CURVE('',#1321,#1320,#736,.T.);
#1577=EDGE_CURVE('',#1318,#1321,#893,.T.);
#1578=EDGE_CURVE('',#1319,#1322,#894,.T.);
#1579=EDGE_CURVE('',#1323,#1322,#895,.T.);
#1580=EDGE_CURVE('',#1320,#1323,#896,.T.);
#1581=EDGE_CURVE('',#1322,#1324,#897,.T.);
#1582=EDGE_CURVE('',#1324,#1325,#898,.T.);
#1583=EDGE_CURVE('',#1323,#1325,#737,.T.);
#1584=EDGE_CURVE('',#1324,#1318,#899,.T.);
#1585=EDGE_CURVE('',#1325,#1321,#900,.T.);
#1586=EDGE_CURVE('',#1326,#1326,#738,.T.);
#1587=EDGE_CURVE('',#1326,#1327,#901,.T.);
#1588=EDGE_CURVE('',#1327,#1327,#739,.T.);
#1589=EDGE_CURVE('',#1328,#1308,#902,.T.);
#1590=EDGE_CURVE('',#1329,#1328,#903,.T.);
#1591=EDGE_CURVE('',#1330,#1329,#904,.T.);
#1592=EDGE_CURVE('',#1330,#1315,#905,.T.);
#1593=EDGE_CURVE('',#1309,#1331,#906,.T.);
#1594=EDGE_CURVE('',#1331,#1328,#907,.T.);
#1595=EDGE_CURVE('',#1332,#1330,#908,.T.);
#1596=EDGE_CURVE('',#1332,#1312,#909,.T.);
#1597=EDGE_CURVE('',#1329,#1333,#910,.T.);
#1598=EDGE_CURVE('',#1333,#1331,#911,.T.);
#1599=EDGE_CURVE('',#1333,#1332,#912,.T.);
#1600=EDGE_CURVE('',#1334,#1334,#740,.T.);
#1601=EDGE_CURVE('',#1334,#1335,#913,.T.);
#1602=EDGE_CURVE('',#1335,#1335,#741,.T.);
#1603=EDGE_CURVE('',#1336,#1336,#742,.T.);
#1604=EDGE_CURVE('',#1336,#1337,#914,.T.);
#1605=EDGE_CURVE('',#1337,#1337,#743,.T.);
#1606=EDGE_CURVE('',#1338,#1339,#915,.T.);
#1607=EDGE_CURVE('',#1339,#1340,#916,.T.);
#1608=EDGE_CURVE('',#1340,#1341,#917,.T.);
#1609=EDGE_CURVE('',#1338,#1341,#918,.T.);
#1610=EDGE_CURVE('',#1339,#1342,#919,.T.);
#1611=EDGE_CURVE('',#1342,#1343,#920,.T.);
#1612=EDGE_CURVE('',#1343,#1340,#921,.T.);
#1613=EDGE_CURVE('',#1342,#1344,#922,.T.);
#1614=EDGE_CURVE('',#1344,#1345,#923,.T.);
#1615=EDGE_CURVE('',#1345,#1343,#924,.T.);
#1616=EDGE_CURVE('',#1344,#1346,#925,.T.);
#1617=EDGE_CURVE('',#1346,#1347,#926,.T.);
#1618=EDGE_CURVE('',#1347,#1345,#927,.T.);
#1619=EDGE_CURVE('',#1346,#1348,#928,.T.);
#1620=EDGE_CURVE('',#1348,#1349,#929,.T.);
#1621=EDGE_CURVE('',#1349,#1347,#930,.T.);
#1622=EDGE_CURVE('',#1348,#1338,#931,.T.);
#1623=EDGE_CURVE('',#1341,#1349,#932,.T.);
#1624=EDGE_CURVE('',#1350,#1350,#744,.T.);
#1625=EDGE_CURVE('',#1351,#1351,#745,.T.);
#1626=EDGE_CURVE('',#1352,#1352,#746,.T.);
#1627=EDGE_CURVE('',#1352,#1351,#933,.T.);
#1628=EDGE_CURVE('',#1353,#1353,#747,.T.);
#1629=EDGE_CURVE('',#1353,#1352,#934,.T.);
#1630=EDGE_CURVE('',#1354,#1354,#748,.T.);
#1631=EDGE_CURVE('',#1354,#1353,#935,.T.);
#1632=EDGE_CURVE('',#1355,#1355,#749,.T.);
#1633=EDGE_CURVE('',#1356,#1356,#750,.F.);
#1634=EDGE_CURVE('',#1356,#1355,#936,.T.);
#1635=EDGE_CURVE('',#1350,#1356,#937,.T.);
#1636=EDGE_CURVE('',#1357,#1357,#751,.T.);
#1637=EDGE_CURVE('',#1357,#1358,#938,.T.);
#1638=EDGE_CURVE('',#1358,#1358,#752,.T.);
#1639=EDGE_CURVE('',#1359,#1359,#753,.T.);
#1640=EDGE_CURVE('',#1359,#1360,#939,.T.);
#1641=EDGE_CURVE('',#1360,#1360,#754,.T.);
#1642=EDGE_CURVE('',#1361,#1362,#940,.T.);
#1643=EDGE_CURVE('',#1363,#1361,#755,.T.);
#1644=EDGE_CURVE('',#1364,#1363,#941,.T.);
#1645=EDGE_CURVE('',#1364,#1362,#756,.T.);
#1646=EDGE_CURVE('',#1362,#1365,#942,.T.);
#1647=EDGE_CURVE('',#1366,#1365,#943,.T.);
#1648=EDGE_CURVE('',#1361,#1366,#944,.T.);
#1649=EDGE_CURVE('',#1367,#1364,#945,.T.);
#1650=EDGE_CURVE('',#1365,#1367,#757,.T.);
#1651=EDGE_CURVE('',#1368,#1363,#946,.T.);
#1652=EDGE_CURVE('',#1367,#1368,#947,.T.);
#1653=EDGE_CURVE('',#1366,#1368,#758,.T.);
#1654=EDGE_CURVE('',#1369,#1369,#759,.T.);
#1655=EDGE_CURVE('',#1369,#1370,#948,.T.);
#1656=EDGE_CURVE('',#1370,#1370,#760,.T.);
#1657=EDGE_CURVE('',#1371,#1371,#761,.T.);
#1658=EDGE_CURVE('',#1371,#1372,#949,.T.);
#1659=EDGE_CURVE('',#1372,#1372,#762,.T.);
#1660=EDGE_CURVE('',#1373,#1373,#763,.T.);
#1661=EDGE_CURVE('',#1373,#1374,#950,.T.);
#1662=EDGE_CURVE('',#1374,#1374,#764,.T.);
#1663=EDGE_CURVE('',#1375,#1376,#951,.T.);
#1664=EDGE_CURVE('',#1377,#1375,#952,.T.);
#1665=EDGE_CURVE('',#1378,#1377,#953,.T.);
#1666=EDGE_CURVE('',#1378,#1376,#954,.T.);
#1667=EDGE_CURVE('',#1379,#1380,#955,.T.);
#1668=EDGE_CURVE('',#1380,#1381,#956,.T.);
#1669=EDGE_CURVE('',#1381,#1382,#957,.T.);
#1670=EDGE_CURVE('',#1382,#1379,#958,.T.);
#1671=EDGE_CURVE('',#1383,#1375,#959,.T.);
#1672=EDGE_CURVE('',#1383,#1380,#960,.T.);
#1673=EDGE_CURVE('',#1384,#1379,#961,.T.);
#1674=EDGE_CURVE('',#1385,#1384,#962,.T.);
#1675=EDGE_CURVE('',#1385,#1386,#963,.T.);
#1676=EDGE_CURVE('',#1377,#1386,#964,.T.);
#1677=EDGE_CURVE('',#1387,#1388,#965,.T.);
#1678=EDGE_CURVE('',#1388,#1385,#966,.T.);
#1679=EDGE_CURVE('',#1384,#1387,#967,.T.);
#1680=EDGE_CURVE('',#1389,#1383,#968,.T.);
#1681=EDGE_CURVE('',#1389,#1381,#969,.T.);
#1682=EDGE_CURVE('',#1387,#1382,#970,.T.);
#1683=EDGE_CURVE('',#1390,#1390,#765,.T.);
#1684=EDGE_CURVE('',#1376,#1389,#971,.T.);
#1685=EDGE_CURVE('',#1391,#1378,#972,.T.);
#1686=EDGE_CURVE('',#1388,#1391,#973,.T.);
#1687=EDGE_CURVE('',#1386,#1391,#974,.T.);
#1688=EDGE_CURVE('',#1392,#1392,#766,.T.);
#1689=EDGE_CURVE('',#1392,#1390,#975,.T.);
#1690=EDGE_CURVE('',#1393,#1393,#767,.F.);
#1691=EDGE_CURVE('',#1393,#1394,#976,.T.);
#1692=EDGE_CURVE('',#1394,#1394,#768,.F.);
#1693=EDGE_CURVE('',#1395,#1395,#769,.T.);
#1694=EDGE_CURVE('',#1395,#1393,#977,.T.);
#1695=EDGE_CURVE('',#1396,#1396,#770,.T.);
#1696=EDGE_CURVE('',#1396,#1397,#978,.T.);
#1697=EDGE_CURVE('',#1398,#1397,#18,.T.);
#1698=EDGE_CURVE('',#1399,#1398,#19,.T.);
#1699=EDGE_CURVE('',#1400,#1399,#20,.T.);
#1700=EDGE_CURVE('',#1401,#1400,#21,.T.);
#1701=EDGE_CURVE('',#1402,#1401,#22,.T.);
#1702=EDGE_CURVE('',#1397,#1402,#23,.T.);
#1703=EDGE_CURVE('',#1403,#1401,#979,.T.);
#1704=EDGE_CURVE('',#1403,#1404,#980,.T.);
#1705=EDGE_CURVE('',#1404,#1402,#981,.T.);
#1706=EDGE_CURVE('',#1405,#1400,#982,.T.);
#1707=EDGE_CURVE('',#1405,#1403,#983,.T.);
#1708=EDGE_CURVE('',#1406,#1399,#984,.T.);
#1709=EDGE_CURVE('',#1406,#1405,#985,.T.);
#1710=EDGE_CURVE('',#1407,#1398,#986,.T.);
#1711=EDGE_CURVE('',#1407,#1406,#987,.T.);
#1712=EDGE_CURVE('',#1408,#1397,#988,.T.);
#1713=EDGE_CURVE('',#1408,#1407,#989,.T.);
#1714=EDGE_CURVE('',#1404,#1408,#990,.T.);
#1715=EDGE_CURVE('',#1409,#1410,#24,.T.);
#1716=EDGE_CURVE('',#1411,#1409,#25,.T.);
#1717=EDGE_CURVE('',#1411,#1412,#991,.T.);
#1718=EDGE_CURVE('',#1412,#1412,#771,.T.);
#1719=EDGE_CURVE('',#1413,#1411,#26,.T.);
#1720=EDGE_CURVE('',#1414,#1413,#27,.T.);
#1721=EDGE_CURVE('',#1415,#1414,#28,.T.);
#1722=EDGE_CURVE('',#1410,#1415,#29,.T.);
#1723=EDGE_CURVE('',#1416,#1416,#772,.T.);
#1724=EDGE_CURVE('',#1416,#1417,#992,.T.);
#1725=EDGE_CURVE('',#1418,#1417,#30,.T.);
#1726=EDGE_CURVE('',#1419,#1418,#31,.T.);
#1727=EDGE_CURVE('',#1420,#1419,#32,.T.);
#1728=EDGE_CURVE('',#1421,#1420,#33,.T.);
#1729=EDGE_CURVE('',#1422,#1421,#34,.T.);
#1730=EDGE_CURVE('',#1417,#1422,#35,.T.);
#1731=EDGE_CURVE('',#1413,#1422,#993,.T.);
#1732=EDGE_CURVE('',#1414,#1421,#994,.T.);
#1733=EDGE_CURVE('',#1411,#1417,#995,.T.);
#1734=EDGE_CURVE('',#1409,#1418,#996,.T.);
#1735=EDGE_CURVE('',#1423,#1423,#773,.F.);
#1736=EDGE_CURVE('',#1423,#1424,#997,.T.);
#1737=EDGE_CURVE('',#1424,#1424,#774,.F.);
#1738=EDGE_CURVE('',#1410,#1419,#998,.T.);
#1739=EDGE_CURVE('',#1415,#1420,#999,.T.);
#1740=EDGE_CURVE('',#1425,#1425,#775,.T.);
#1741=EDGE_CURVE('',#1425,#1426,#1000,.T.);
#1742=EDGE_CURVE('',#1426,#1426,#776,.T.);
#1743=EDGE_CURVE('',#1427,#1428,#12,.T.);
#1744=EDGE_CURVE('',#1427,#1429,#1001,.T.);
#1745=EDGE_CURVE('',#1429,#1429,#13,.T.);
#1746=EDGE_CURVE('',#1430,#1427,#14,.T.);
#1747=EDGE_CURVE('',#1428,#1430,#15,.T.);
#1748=EDGE_CURVE('',#1431,#1431,#777,.T.);
#1749=EDGE_CURVE('',#1432,#1432,#778,.T.);
#1750=EDGE_CURVE('',#1432,#1431,#1002,.T.);
#1751=EDGE_CURVE('',#1433,#1433,#779,.T.);
#1752=EDGE_CURVE('',#1433,#1432,#1003,.T.);
#1753=EDGE_CURVE('',#1434,#1434,#780,.T.);
#1754=EDGE_CURVE('',#1435,#1435,#781,.T.);
#1755=EDGE_CURVE('',#1435,#1428,#1004,.T.);
#1756=EDGE_CURVE('',#1430,#1434,#1005,.T.);
#1757=EDGE_CURVE('',#1436,#1436,#782,.T.);
#1758=EDGE_CURVE('',#1436,#1435,#1006,.T.);
#1759=EDGE_CURVE('',#1437,#1437,#783,.T.);
#1760=EDGE_CURVE('',#1437,#1438,#1007,.T.);
#1761=EDGE_CURVE('',#1438,#1438,#784,.T.);
#1762=EDGE_CURVE('',#1439,#1439,#785,.T.);
#1763=EDGE_CURVE('',#1439,#1440,#1008,.T.);
#1764=EDGE_CURVE('',#1440,#1440,#786,.T.);
#1765=EDGE_CURVE('',#1441,#1441,#787,.T.);
#1766=EDGE_CURVE('',#1441,#1442,#1009,.T.);
#1767=EDGE_CURVE('',#1442,#1442,#788,.T.);
#1768=EDGE_CURVE('',#1443,#1443,#789,.T.);
#1769=EDGE_CURVE('',#1443,#1444,#1010,.T.);
#1770=EDGE_CURVE('',#1444,#1444,#790,.T.);
#1771=EDGE_CURVE('',#1445,#1445,#791,.T.);
#1772=EDGE_CURVE('',#1445,#1445,#792,.T.);
#1773=EDGE_CURVE('',#1446,#1447,#16,.T.);
#1774=EDGE_CURVE('',#1447,#1446,#17,.T.);
#1775=EDGE_CURVE('',#1448,#1449,#793,.T.);
#1776=EDGE_CURVE('',#1448,#1449,#1011,.T.);
#1777=EDGE_CURVE('',#1449,#1450,#1012,.T.);
#1778=EDGE_CURVE('',#1451,#1450,#1013,.T.);
#1779=EDGE_CURVE('',#1448,#1451,#1014,.T.);
#1780=EDGE_CURVE('',#1452,#1451,#794,.T.);
#1781=EDGE_CURVE('',#1452,#1447,#1015,.T.);
#1782=EDGE_CURVE('',#1450,#1452,#795,.T.);
#1783=ORIENTED_EDGE('',*,*,#1453,.F.);
#1784=ORIENTED_EDGE('',*,*,#1454,.F.);
#1785=ORIENTED_EDGE('',*,*,#1455,.T.);
#1786=ORIENTED_EDGE('',*,*,#1456,.F.);
#1787=ORIENTED_EDGE('',*,*,#1457,.T.);
#1788=ORIENTED_EDGE('',*,*,#1458,.T.);
#1789=ORIENTED_EDGE('',*,*,#1457,.F.);
#1790=ORIENTED_EDGE('',*,*,#1459,.F.);
#1791=ORIENTED_EDGE('',*,*,#1458,.F.);
#1792=ORIENTED_EDGE('',*,*,#1460,.T.);
#1793=ORIENTED_EDGE('',*,*,#1461,.T.);
#1794=ORIENTED_EDGE('',*,*,#1462,.F.);
#1795=ORIENTED_EDGE('',*,*,#1463,.F.);
#1796=ORIENTED_EDGE('',*,*,#1464,.T.);
#1797=ORIENTED_EDGE('',*,*,#1465,.T.);
#1798=ORIENTED_EDGE('',*,*,#1466,.F.);
#1799=ORIENTED_EDGE('',*,*,#1467,.T.);
#1800=ORIENTED_EDGE('',*,*,#1468,.T.);
#1801=ORIENTED_EDGE('',*,*,#1459,.T.);
#1802=ORIENTED_EDGE('',*,*,#1456,.T.);
#1803=ORIENTED_EDGE('',*,*,#1469,.F.);
#1804=ORIENTED_EDGE('',*,*,#1470,.F.);
#1805=ORIENTED_EDGE('',*,*,#1453,.T.);
#1806=ORIENTED_EDGE('',*,*,#1468,.F.);
#1807=ORIENTED_EDGE('',*,*,#1471,.F.);
#1808=ORIENTED_EDGE('',*,*,#1472,.T.);
#1809=ORIENTED_EDGE('',*,*,#1460,.F.);
#1810=ORIENTED_EDGE('',*,*,#1455,.F.);
#1811=ORIENTED_EDGE('',*,*,#1473,.F.);
#1812=ORIENTED_EDGE('',*,*,#1474,.F.);
#1813=ORIENTED_EDGE('',*,*,#1461,.F.);
#1814=ORIENTED_EDGE('',*,*,#1472,.F.);
#1815=ORIENTED_EDGE('',*,*,#1469,.T.);
#1816=ORIENTED_EDGE('',*,*,#1467,.F.);
#1817=ORIENTED_EDGE('',*,*,#1475,.F.);
#1818=ORIENTED_EDGE('',*,*,#1476,.F.);
#1819=ORIENTED_EDGE('',*,*,#1454,.T.);
#1820=ORIENTED_EDGE('',*,*,#1470,.T.);
#1821=ORIENTED_EDGE('',*,*,#1476,.T.);
#1822=ORIENTED_EDGE('',*,*,#1477,.F.);
#1823=ORIENTED_EDGE('',*,*,#1473,.T.);
#1824=ORIENTED_EDGE('',*,*,#1471,.T.);
#1825=ORIENTED_EDGE('',*,*,#1474,.T.);
#1826=ORIENTED_EDGE('',*,*,#1477,.T.);
#1827=ORIENTED_EDGE('',*,*,#1475,.T.);
#1828=ORIENTED_EDGE('',*,*,#1466,.T.);
#1829=ORIENTED_EDGE('',*,*,#1478,.T.);
#1830=ORIENTED_EDGE('',*,*,#1479,.T.);
#1831=ORIENTED_EDGE('',*,*,#1480,.T.);
#1832=ORIENTED_EDGE('',*,*,#1462,.T.);
#1833=ORIENTED_EDGE('',*,*,#1481,.T.);
#1834=ORIENTED_EDGE('',*,*,#1482,.T.);
#1835=ORIENTED_EDGE('',*,*,#1483,.T.);
#1836=ORIENTED_EDGE('',*,*,#1484,.T.);
#1837=ORIENTED_EDGE('',*,*,#1485,.T.);
#1838=ORIENTED_EDGE('',*,*,#1486,.T.);
#1839=ORIENTED_EDGE('',*,*,#1487,.T.);
#1840=ORIENTED_EDGE('',*,*,#1488,.T.);
#1841=ORIENTED_EDGE('',*,*,#1489,.T.);
#1842=ORIENTED_EDGE('',*,*,#1490,.T.);
#1843=ORIENTED_EDGE('',*,*,#1491,.T.);
#1844=ORIENTED_EDGE('',*,*,#1492,.T.);
#1845=ORIENTED_EDGE('',*,*,#1493,.T.);
#1846=ORIENTED_EDGE('',*,*,#1494,.T.);
#1847=ORIENTED_EDGE('',*,*,#1495,.F.);
#1848=ORIENTED_EDGE('',*,*,#1496,.T.);
#1849=ORIENTED_EDGE('',*,*,#1494,.F.);
#1850=ORIENTED_EDGE('',*,*,#1496,.F.);
#1851=ORIENTED_EDGE('',*,*,#1497,.F.);
#1852=ORIENTED_EDGE('',*,*,#1498,.T.);
#1853=ORIENTED_EDGE('',*,*,#1493,.F.);
#1854=ORIENTED_EDGE('',*,*,#1498,.F.);
#1855=ORIENTED_EDGE('',*,*,#1499,.F.);
#1856=ORIENTED_EDGE('',*,*,#1500,.T.);
#1857=ORIENTED_EDGE('',*,*,#1501,.F.);
#1858=ORIENTED_EDGE('',*,*,#1500,.F.);
#1859=ORIENTED_EDGE('',*,*,#1490,.F.);
#1860=ORIENTED_EDGE('',*,*,#1502,.T.);
#1861=ORIENTED_EDGE('',*,*,#1503,.T.);
#1862=ORIENTED_EDGE('',*,*,#1504,.T.);
#1863=ORIENTED_EDGE('',*,*,#1489,.F.);
#1864=ORIENTED_EDGE('',*,*,#1505,.F.);
#1865=ORIENTED_EDGE('',*,*,#1506,.F.);
#1866=ORIENTED_EDGE('',*,*,#1502,.F.);
#1867=ORIENTED_EDGE('',*,*,#1501,.T.);
#1868=ORIENTED_EDGE('',*,*,#1491,.F.);
#1869=ORIENTED_EDGE('',*,*,#1504,.F.);
#1870=ORIENTED_EDGE('',*,*,#1507,.T.);
#1871=ORIENTED_EDGE('',*,*,#1508,.F.);
#1872=ORIENTED_EDGE('',*,*,#1499,.T.);
#1873=ORIENTED_EDGE('',*,*,#1503,.F.);
#1874=ORIENTED_EDGE('',*,*,#1506,.T.);
#1875=ORIENTED_EDGE('',*,*,#1509,.F.);
#1876=ORIENTED_EDGE('',*,*,#1507,.F.);
#1877=ORIENTED_EDGE('',*,*,#1492,.F.);
#1878=ORIENTED_EDGE('',*,*,#1508,.T.);
#1879=ORIENTED_EDGE('',*,*,#1509,.T.);
#1880=ORIENTED_EDGE('',*,*,#1505,.T.);
#1881=ORIENTED_EDGE('',*,*,#1510,.F.);
#1882=ORIENTED_EDGE('',*,*,#1511,.T.);
#1883=ORIENTED_EDGE('',*,*,#1512,.F.);
#1884=ORIENTED_EDGE('',*,*,#1511,.F.);
#1885=ORIENTED_EDGE('',*,*,#1513,.F.);
#1886=ORIENTED_EDGE('',*,*,#1514,.T.);
#1887=ORIENTED_EDGE('',*,*,#1515,.F.);
#1888=ORIENTED_EDGE('',*,*,#1514,.F.);
#1889=ORIENTED_EDGE('',*,*,#1486,.F.);
#1890=ORIENTED_EDGE('',*,*,#1516,.T.);
#1891=ORIENTED_EDGE('',*,*,#1517,.T.);
#1892=ORIENTED_EDGE('',*,*,#1518,.T.);
#1893=ORIENTED_EDGE('',*,*,#1513,.T.);
#1894=ORIENTED_EDGE('',*,*,#1485,.F.);
#1895=ORIENTED_EDGE('',*,*,#1519,.F.);
#1896=ORIENTED_EDGE('',*,*,#1520,.F.);
#1897=ORIENTED_EDGE('',*,*,#1516,.F.);
#1898=ORIENTED_EDGE('',*,*,#1487,.F.);
#1899=ORIENTED_EDGE('',*,*,#1518,.F.);
#1900=ORIENTED_EDGE('',*,*,#1521,.T.);
#1901=ORIENTED_EDGE('',*,*,#1522,.F.);
#1902=ORIENTED_EDGE('',*,*,#1517,.F.);
#1903=ORIENTED_EDGE('',*,*,#1520,.T.);
#1904=ORIENTED_EDGE('',*,*,#1523,.F.);
#1905=ORIENTED_EDGE('',*,*,#1521,.F.);
#1906=ORIENTED_EDGE('',*,*,#1488,.F.);
#1907=ORIENTED_EDGE('',*,*,#1522,.T.);
#1908=ORIENTED_EDGE('',*,*,#1523,.T.);
#1909=ORIENTED_EDGE('',*,*,#1519,.T.);
#1910=ORIENTED_EDGE('',*,*,#1515,.T.);
#1911=ORIENTED_EDGE('',*,*,#1482,.F.);
#1912=ORIENTED_EDGE('',*,*,#1524,.T.);
#1913=ORIENTED_EDGE('',*,*,#1525,.T.);
#1914=ORIENTED_EDGE('',*,*,#1526,.T.);
#1915=ORIENTED_EDGE('',*,*,#1510,.T.);
#1916=ORIENTED_EDGE('',*,*,#1481,.F.);
#1917=ORIENTED_EDGE('',*,*,#1527,.F.);
#1918=ORIENTED_EDGE('',*,*,#1528,.F.);
#1919=ORIENTED_EDGE('',*,*,#1524,.F.);
#1920=ORIENTED_EDGE('',*,*,#1483,.F.);
#1921=ORIENTED_EDGE('',*,*,#1526,.F.);
#1922=ORIENTED_EDGE('',*,*,#1529,.T.);
#1923=ORIENTED_EDGE('',*,*,#1530,.F.);
#1924=ORIENTED_EDGE('',*,*,#1525,.F.);
#1925=ORIENTED_EDGE('',*,*,#1528,.T.);
#1926=ORIENTED_EDGE('',*,*,#1531,.F.);
#1927=ORIENTED_EDGE('',*,*,#1529,.F.);
#1928=ORIENTED_EDGE('',*,*,#1484,.F.);
#1929=ORIENTED_EDGE('',*,*,#1530,.T.);
#1930=ORIENTED_EDGE('',*,*,#1531,.T.);
#1931=ORIENTED_EDGE('',*,*,#1527,.T.);
#1932=ORIENTED_EDGE('',*,*,#1512,.T.);
#1933=ORIENTED_EDGE('',*,*,#1532,.T.);
#1934=ORIENTED_EDGE('',*,*,#1463,.T.);
#1935=ORIENTED_EDGE('',*,*,#1480,.F.);
#1936=ORIENTED_EDGE('',*,*,#1533,.F.);
#1937=ORIENTED_EDGE('',*,*,#1534,.T.);
#1938=ORIENTED_EDGE('',*,*,#1533,.T.);
#1939=ORIENTED_EDGE('',*,*,#1479,.F.);
#1940=ORIENTED_EDGE('',*,*,#1535,.F.);
#1941=ORIENTED_EDGE('',*,*,#1536,.T.);
#1942=ORIENTED_EDGE('',*,*,#1535,.T.);
#1943=ORIENTED_EDGE('',*,*,#1478,.F.);
#1944=ORIENTED_EDGE('',*,*,#1465,.F.);
#1945=ORIENTED_EDGE('',*,*,#1536,.F.);
#1946=ORIENTED_EDGE('',*,*,#1464,.F.);
#1947=ORIENTED_EDGE('',*,*,#1532,.F.);
#1948=ORIENTED_EDGE('',*,*,#1534,.F.);
#1949=ORIENTED_EDGE('',*,*,#1495,.T.);
#1950=ORIENTED_EDGE('',*,*,#1497,.T.);
#1951=ORIENTED_EDGE('',*,*,#1537,.F.);
#1952=ORIENTED_EDGE('',*,*,#1538,.T.);
#1953=ORIENTED_EDGE('',*,*,#1539,.F.);
#1954=ORIENTED_EDGE('',*,*,#1538,.F.);
#1955=ORIENTED_EDGE('',*,*,#1540,.F.);
#1956=ORIENTED_EDGE('',*,*,#1541,.T.);
#1957=ORIENTED_EDGE('',*,*,#1542,.F.);
#1958=ORIENTED_EDGE('',*,*,#1541,.F.);
#1959=ORIENTED_EDGE('',*,*,#1543,.F.);
#1960=ORIENTED_EDGE('',*,*,#1544,.F.);
#1961=ORIENTED_EDGE('',*,*,#1545,.F.);
#1962=ORIENTED_EDGE('',*,*,#1546,.T.);
#1963=ORIENTED_EDGE('',*,*,#1546,.F.);
#1964=ORIENTED_EDGE('',*,*,#1547,.F.);
#1965=ORIENTED_EDGE('',*,*,#1548,.F.);
#1966=ORIENTED_EDGE('',*,*,#1549,.F.);
#1967=ORIENTED_EDGE('',*,*,#1537,.T.);
#1968=ORIENTED_EDGE('',*,*,#1545,.T.);
#1969=ORIENTED_EDGE('',*,*,#1550,.F.);
#1970=ORIENTED_EDGE('',*,*,#1551,.F.);
#1971=ORIENTED_EDGE('',*,*,#1547,.T.);
#1972=ORIENTED_EDGE('',*,*,#1552,.T.);
#1973=ORIENTED_EDGE('',*,*,#1553,.F.);
#1974=ORIENTED_EDGE('',*,*,#1550,.T.);
#1975=ORIENTED_EDGE('',*,*,#1544,.T.);
#1976=ORIENTED_EDGE('',*,*,#1539,.T.);
#1977=ORIENTED_EDGE('',*,*,#1543,.T.);
#1978=ORIENTED_EDGE('',*,*,#1549,.T.);
#1979=ORIENTED_EDGE('',*,*,#1554,.F.);
#1980=ORIENTED_EDGE('',*,*,#1552,.F.);
#1981=ORIENTED_EDGE('',*,*,#1555,.F.);
#1982=ORIENTED_EDGE('',*,*,#1556,.T.);
#1983=ORIENTED_EDGE('',*,*,#1557,.F.);
#1984=ORIENTED_EDGE('',*,*,#1556,.F.);
#1985=ORIENTED_EDGE('',*,*,#1558,.F.);
#1986=ORIENTED_EDGE('',*,*,#1559,.T.);
#1987=ORIENTED_EDGE('',*,*,#1560,.F.);
#1988=ORIENTED_EDGE('',*,*,#1559,.F.);
#1989=ORIENTED_EDGE('',*,*,#1561,.F.);
#1990=ORIENTED_EDGE('',*,*,#1562,.T.);
#1991=ORIENTED_EDGE('',*,*,#1563,.F.);
#1992=ORIENTED_EDGE('',*,*,#1564,.F.);
#1993=ORIENTED_EDGE('',*,*,#1565,.T.);
#1994=ORIENTED_EDGE('',*,*,#1566,.T.);
#1995=ORIENTED_EDGE('',*,*,#1567,.T.);
#1996=ORIENTED_EDGE('',*,*,#1568,.T.);
#1997=ORIENTED_EDGE('',*,*,#1560,.T.);
#1998=ORIENTED_EDGE('',*,*,#1569,.F.);
#1999=ORIENTED_EDGE('',*,*,#1570,.T.);
#2000=ORIENTED_EDGE('',*,*,#1566,.F.);
#2001=ORIENTED_EDGE('',*,*,#1571,.F.);
#2002=ORIENTED_EDGE('',*,*,#1563,.T.);
#2003=ORIENTED_EDGE('',*,*,#1572,.T.);
#2004=ORIENTED_EDGE('',*,*,#1569,.T.);
#2005=ORIENTED_EDGE('',*,*,#1573,.T.);
#2006=ORIENTED_EDGE('',*,*,#1558,.T.);
#2007=ORIENTED_EDGE('',*,*,#1574,.T.);
#2008=ORIENTED_EDGE('',*,*,#1575,.F.);
#2009=ORIENTED_EDGE('',*,*,#1576,.F.);
#2010=ORIENTED_EDGE('',*,*,#1577,.F.);
#2011=ORIENTED_EDGE('',*,*,#1578,.T.);
#2012=ORIENTED_EDGE('',*,*,#1579,.F.);
#2013=ORIENTED_EDGE('',*,*,#1580,.F.);
#2014=ORIENTED_EDGE('',*,*,#1575,.T.);
#2015=ORIENTED_EDGE('',*,*,#1581,.T.);
#2016=ORIENTED_EDGE('',*,*,#1582,.T.);
#2017=ORIENTED_EDGE('',*,*,#1583,.F.);
#2018=ORIENTED_EDGE('',*,*,#1579,.T.);
#2019=ORIENTED_EDGE('',*,*,#1584,.T.);
#2020=ORIENTED_EDGE('',*,*,#1577,.T.);
#2021=ORIENTED_EDGE('',*,*,#1585,.F.);
#2022=ORIENTED_EDGE('',*,*,#1582,.F.);
#2023=ORIENTED_EDGE('',*,*,#1586,.F.);
#2024=ORIENTED_EDGE('',*,*,#1587,.T.);
#2025=ORIENTED_EDGE('',*,*,#1588,.T.);
#2026=ORIENTED_EDGE('',*,*,#1587,.F.);
#2027=ORIENTED_EDGE('',*,*,#1551,.T.);
#2028=ORIENTED_EDGE('',*,*,#1553,.T.);
#2029=ORIENTED_EDGE('',*,*,#1554,.T.);
#2030=ORIENTED_EDGE('',*,*,#1548,.T.);
#2031=ORIENTED_EDGE('',*,*,#1580,.T.);
#2032=ORIENTED_EDGE('',*,*,#1583,.T.);
#2033=ORIENTED_EDGE('',*,*,#1585,.T.);
#2034=ORIENTED_EDGE('',*,*,#1576,.T.);
#2035=ORIENTED_EDGE('',*,*,#1586,.T.);
#2036=ORIENTED_EDGE('',*,*,#1542,.T.);
#2037=ORIENTED_EDGE('',*,*,#1588,.F.);
#2038=ORIENTED_EDGE('',*,*,#1540,.T.);
#2039=ORIENTED_EDGE('',*,*,#1589,.F.);
#2040=ORIENTED_EDGE('',*,*,#1590,.F.);
#2041=ORIENTED_EDGE('',*,*,#1591,.F.);
#2042=ORIENTED_EDGE('',*,*,#1592,.T.);
#2043=ORIENTED_EDGE('',*,*,#1567,.F.);
#2044=ORIENTED_EDGE('',*,*,#1570,.F.);
#2045=ORIENTED_EDGE('',*,*,#1572,.F.);
#2046=ORIENTED_EDGE('',*,*,#1562,.F.);
#2047=ORIENTED_EDGE('',*,*,#1561,.T.);
#2048=ORIENTED_EDGE('',*,*,#1593,.T.);
#2049=ORIENTED_EDGE('',*,*,#1594,.T.);
#2050=ORIENTED_EDGE('',*,*,#1589,.T.);
#2051=ORIENTED_EDGE('',*,*,#1557,.T.);
#2052=ORIENTED_EDGE('',*,*,#1595,.F.);
#2053=ORIENTED_EDGE('',*,*,#1596,.T.);
#2054=ORIENTED_EDGE('',*,*,#1568,.F.);
#2055=ORIENTED_EDGE('',*,*,#1592,.F.);
#2056=ORIENTED_EDGE('',*,*,#1581,.F.);
#2057=ORIENTED_EDGE('',*,*,#1578,.F.);
#2058=ORIENTED_EDGE('',*,*,#1574,.F.);
#2059=ORIENTED_EDGE('',*,*,#1584,.F.);
#2060=ORIENTED_EDGE('',*,*,#1597,.F.);
#2061=ORIENTED_EDGE('',*,*,#1590,.T.);
#2062=ORIENTED_EDGE('',*,*,#1594,.F.);
#2063=ORIENTED_EDGE('',*,*,#1598,.F.);
#2064=ORIENTED_EDGE('',*,*,#1599,.F.);
#2065=ORIENTED_EDGE('',*,*,#1598,.T.);
#2066=ORIENTED_EDGE('',*,*,#1593,.F.);
#2067=ORIENTED_EDGE('',*,*,#1564,.T.);
#2068=ORIENTED_EDGE('',*,*,#1573,.F.);
#2069=ORIENTED_EDGE('',*,*,#1571,.T.);
#2070=ORIENTED_EDGE('',*,*,#1565,.F.);
#2071=ORIENTED_EDGE('',*,*,#1596,.F.);
#2072=ORIENTED_EDGE('',*,*,#1591,.T.);
#2073=ORIENTED_EDGE('',*,*,#1597,.T.);
#2074=ORIENTED_EDGE('',*,*,#1599,.T.);
#2075=ORIENTED_EDGE('',*,*,#1595,.T.);
#2076=ORIENTED_EDGE('',*,*,#1555,.T.);
#2077=ORIENTED_EDGE('',*,*,#1600,.F.);
#2078=ORIENTED_EDGE('',*,*,#1601,.T.);
#2079=ORIENTED_EDGE('',*,*,#1602,.F.);
#2080=ORIENTED_EDGE('',*,*,#1601,.F.);
#2081=ORIENTED_EDGE('',*,*,#1600,.T.);
#2082=ORIENTED_EDGE('',*,*,#1603,.F.);
#2083=ORIENTED_EDGE('',*,*,#1604,.T.);
#2084=ORIENTED_EDGE('',*,*,#1605,.T.);
#2085=ORIENTED_EDGE('',*,*,#1604,.F.);
#2086=ORIENTED_EDGE('',*,*,#1603,.T.);
#2087=ORIENTED_EDGE('',*,*,#1602,.T.);
#2088=ORIENTED_EDGE('',*,*,#1605,.F.);
#2089=ORIENTED_EDGE('',*,*,#1606,.T.);
#2090=ORIENTED_EDGE('',*,*,#1607,.T.);
#2091=ORIENTED_EDGE('',*,*,#1608,.T.);
#2092=ORIENTED_EDGE('',*,*,#1609,.F.);
#2093=ORIENTED_EDGE('',*,*,#1610,.T.);
#2094=ORIENTED_EDGE('',*,*,#1611,.T.);
#2095=ORIENTED_EDGE('',*,*,#1612,.T.);
#2096=ORIENTED_EDGE('',*,*,#1607,.F.);
#2097=ORIENTED_EDGE('',*,*,#1613,.T.);
#2098=ORIENTED_EDGE('',*,*,#1614,.T.);
#2099=ORIENTED_EDGE('',*,*,#1615,.T.);
#2100=ORIENTED_EDGE('',*,*,#1611,.F.);
#2101=ORIENTED_EDGE('',*,*,#1616,.T.);
#2102=ORIENTED_EDGE('',*,*,#1617,.T.);
#2103=ORIENTED_EDGE('',*,*,#1618,.T.);
#2104=ORIENTED_EDGE('',*,*,#1614,.F.);
#2105=ORIENTED_EDGE('',*,*,#1619,.T.);
#2106=ORIENTED_EDGE('',*,*,#1620,.T.);
#2107=ORIENTED_EDGE('',*,*,#1621,.T.);
#2108=ORIENTED_EDGE('',*,*,#1617,.F.);
#2109=ORIENTED_EDGE('',*,*,#1622,.T.);
#2110=ORIENTED_EDGE('',*,*,#1609,.T.);
#2111=ORIENTED_EDGE('',*,*,#1623,.T.);
#2112=ORIENTED_EDGE('',*,*,#1620,.F.);
#2113=ORIENTED_EDGE('',*,*,#1622,.F.);
#2114=ORIENTED_EDGE('',*,*,#1619,.F.);
#2115=ORIENTED_EDGE('',*,*,#1616,.F.);
#2116=ORIENTED_EDGE('',*,*,#1613,.F.);
#2117=ORIENTED_EDGE('',*,*,#1610,.F.);
#2118=ORIENTED_EDGE('',*,*,#1606,.F.);
#2119=ORIENTED_EDGE('',*,*,#1623,.F.);
#2120=ORIENTED_EDGE('',*,*,#1608,.F.);
#2121=ORIENTED_EDGE('',*,*,#1612,.F.);
#2122=ORIENTED_EDGE('',*,*,#1615,.F.);
#2123=ORIENTED_EDGE('',*,*,#1618,.F.);
#2124=ORIENTED_EDGE('',*,*,#1621,.F.);
#2125=ORIENTED_EDGE('',*,*,#1624,.F.);
#2126=ORIENTED_EDGE('',*,*,#1625,.F.);
#2127=ORIENTED_EDGE('',*,*,#1626,.F.);
#2128=ORIENTED_EDGE('',*,*,#1627,.T.);
#2129=ORIENTED_EDGE('',*,*,#1625,.T.);
#2130=ORIENTED_EDGE('',*,*,#1627,.F.);
#2131=ORIENTED_EDGE('',*,*,#1628,.F.);
#2132=ORIENTED_EDGE('',*,*,#1629,.T.);
#2133=ORIENTED_EDGE('',*,*,#1626,.T.);
#2134=ORIENTED_EDGE('',*,*,#1629,.F.);
#2135=ORIENTED_EDGE('',*,*,#1630,.F.);
#2136=ORIENTED_EDGE('',*,*,#1631,.T.);
#2137=ORIENTED_EDGE('',*,*,#1628,.T.);
#2138=ORIENTED_EDGE('',*,*,#1631,.F.);
#2139=ORIENTED_EDGE('',*,*,#1630,.T.);
#2140=ORIENTED_EDGE('',*,*,#1632,.F.);
#2141=ORIENTED_EDGE('',*,*,#1633,.F.);
#2142=ORIENTED_EDGE('',*,*,#1634,.T.);
#2143=ORIENTED_EDGE('',*,*,#1632,.T.);
#2144=ORIENTED_EDGE('',*,*,#1634,.F.);
#2145=ORIENTED_EDGE('',*,*,#1624,.T.);
#2146=ORIENTED_EDGE('',*,*,#1635,.T.);
#2147=ORIENTED_EDGE('',*,*,#1633,.T.);
#2148=ORIENTED_EDGE('',*,*,#1635,.F.);
#2149=ORIENTED_EDGE('',*,*,#1636,.F.);
#2150=ORIENTED_EDGE('',*,*,#1637,.T.);
#2151=ORIENTED_EDGE('',*,*,#1638,.F.);
#2152=ORIENTED_EDGE('',*,*,#1637,.F.);
#2153=ORIENTED_EDGE('',*,*,#1639,.F.);
#2154=ORIENTED_EDGE('',*,*,#1640,.T.);
#2155=ORIENTED_EDGE('',*,*,#1641,.F.);
#2156=ORIENTED_EDGE('',*,*,#1640,.F.);
#2157=ORIENTED_EDGE('',*,*,#1642,.F.);
#2158=ORIENTED_EDGE('',*,*,#1643,.F.);
#2159=ORIENTED_EDGE('',*,*,#1644,.F.);
#2160=ORIENTED_EDGE('',*,*,#1645,.T.);
#2161=ORIENTED_EDGE('',*,*,#1642,.T.);
#2162=ORIENTED_EDGE('',*,*,#1646,.T.);
#2163=ORIENTED_EDGE('',*,*,#1647,.F.);
#2164=ORIENTED_EDGE('',*,*,#1648,.F.);
#2165=ORIENTED_EDGE('',*,*,#1645,.F.);
#2166=ORIENTED_EDGE('',*,*,#1649,.F.);
#2167=ORIENTED_EDGE('',*,*,#1650,.F.);
#2168=ORIENTED_EDGE('',*,*,#1646,.F.);
#2169=ORIENTED_EDGE('',*,*,#1636,.T.);
#2170=ORIENTED_EDGE('',*,*,#1639,.T.);
#2171=ORIENTED_EDGE('',*,*,#1644,.T.);
#2172=ORIENTED_EDGE('',*,*,#1651,.F.);
#2173=ORIENTED_EDGE('',*,*,#1652,.F.);
#2174=ORIENTED_EDGE('',*,*,#1649,.T.);
#2175=ORIENTED_EDGE('',*,*,#1647,.T.);
#2176=ORIENTED_EDGE('',*,*,#1650,.T.);
#2177=ORIENTED_EDGE('',*,*,#1652,.T.);
#2178=ORIENTED_EDGE('',*,*,#1653,.F.);
#2179=ORIENTED_EDGE('',*,*,#1648,.T.);
#2180=ORIENTED_EDGE('',*,*,#1653,.T.);
#2181=ORIENTED_EDGE('',*,*,#1651,.T.);
#2182=ORIENTED_EDGE('',*,*,#1643,.T.);
#2183=ORIENTED_EDGE('',*,*,#1638,.T.);
#2184=ORIENTED_EDGE('',*,*,#1641,.T.);
#2185=ORIENTED_EDGE('',*,*,#1654,.F.);
#2186=ORIENTED_EDGE('',*,*,#1655,.T.);
#2187=ORIENTED_EDGE('',*,*,#1656,.F.);
#2188=ORIENTED_EDGE('',*,*,#1655,.F.);
#2189=ORIENTED_EDGE('',*,*,#1654,.T.);
#2190=ORIENTED_EDGE('',*,*,#1657,.F.);
#2191=ORIENTED_EDGE('',*,*,#1658,.T.);
#2192=ORIENTED_EDGE('',*,*,#1659,.F.);
#2193=ORIENTED_EDGE('',*,*,#1658,.F.);
#2194=ORIENTED_EDGE('',*,*,#1660,.F.);
#2195=ORIENTED_EDGE('',*,*,#1661,.T.);
#2196=ORIENTED_EDGE('',*,*,#1662,.F.);
#2197=ORIENTED_EDGE('',*,*,#1661,.F.);
#2198=ORIENTED_EDGE('',*,*,#1663,.F.);
#2199=ORIENTED_EDGE('',*,*,#1664,.F.);
#2200=ORIENTED_EDGE('',*,*,#1665,.F.);
#2201=ORIENTED_EDGE('',*,*,#1666,.T.);
#2202=ORIENTED_EDGE('',*,*,#1667,.T.);
#2203=ORIENTED_EDGE('',*,*,#1668,.T.);
#2204=ORIENTED_EDGE('',*,*,#1669,.T.);
#2205=ORIENTED_EDGE('',*,*,#1670,.T.);
#2206=ORIENTED_EDGE('',*,*,#1662,.T.);
#2207=ORIENTED_EDGE('',*,*,#1671,.F.);
#2208=ORIENTED_EDGE('',*,*,#1672,.T.);
#2209=ORIENTED_EDGE('',*,*,#1667,.F.);
#2210=ORIENTED_EDGE('',*,*,#1673,.F.);
#2211=ORIENTED_EDGE('',*,*,#1674,.F.);
#2212=ORIENTED_EDGE('',*,*,#1675,.T.);
#2213=ORIENTED_EDGE('',*,*,#1676,.F.);
#2214=ORIENTED_EDGE('',*,*,#1664,.T.);
#2215=ORIENTED_EDGE('',*,*,#1677,.T.);
#2216=ORIENTED_EDGE('',*,*,#1678,.T.);
#2217=ORIENTED_EDGE('',*,*,#1674,.T.);
#2218=ORIENTED_EDGE('',*,*,#1679,.T.);
#2219=ORIENTED_EDGE('',*,*,#1657,.T.);
#2220=ORIENTED_EDGE('',*,*,#1680,.F.);
#2221=ORIENTED_EDGE('',*,*,#1681,.T.);
#2222=ORIENTED_EDGE('',*,*,#1668,.F.);
#2223=ORIENTED_EDGE('',*,*,#1672,.F.);
#2224=ORIENTED_EDGE('',*,*,#1673,.T.);
#2225=ORIENTED_EDGE('',*,*,#1670,.F.);
#2226=ORIENTED_EDGE('',*,*,#1682,.F.);
#2227=ORIENTED_EDGE('',*,*,#1679,.F.);
#2228=ORIENTED_EDGE('',*,*,#1683,.F.);
#2229=ORIENTED_EDGE('',*,*,#1669,.F.);
#2230=ORIENTED_EDGE('',*,*,#1681,.F.);
#2231=ORIENTED_EDGE('',*,*,#1684,.F.);
#2232=ORIENTED_EDGE('',*,*,#1666,.F.);
#2233=ORIENTED_EDGE('',*,*,#1685,.F.);
#2234=ORIENTED_EDGE('',*,*,#1686,.F.);
#2235=ORIENTED_EDGE('',*,*,#1677,.F.);
#2236=ORIENTED_EDGE('',*,*,#1682,.T.);
#2237=ORIENTED_EDGE('',*,*,#1663,.T.);
#2238=ORIENTED_EDGE('',*,*,#1684,.T.);
#2239=ORIENTED_EDGE('',*,*,#1680,.T.);
#2240=ORIENTED_EDGE('',*,*,#1671,.T.);
#2241=ORIENTED_EDGE('',*,*,#1660,.T.);
#2242=ORIENTED_EDGE('',*,*,#1678,.F.);
#2243=ORIENTED_EDGE('',*,*,#1686,.T.);
#2244=ORIENTED_EDGE('',*,*,#1687,.F.);
#2245=ORIENTED_EDGE('',*,*,#1675,.F.);
#2246=ORIENTED_EDGE('',*,*,#1665,.T.);
#2247=ORIENTED_EDGE('',*,*,#1676,.T.);
#2248=ORIENTED_EDGE('',*,*,#1687,.T.);
#2249=ORIENTED_EDGE('',*,*,#1685,.T.);
#2250=ORIENTED_EDGE('',*,*,#1659,.T.);
#2251=ORIENTED_EDGE('',*,*,#1688,.F.);
#2252=ORIENTED_EDGE('',*,*,#1689,.T.);
#2253=ORIENTED_EDGE('',*,*,#1683,.T.);
#2254=ORIENTED_EDGE('',*,*,#1689,.F.);
#2255=ORIENTED_EDGE('',*,*,#1688,.T.);
#2256=ORIENTED_EDGE('',*,*,#1656,.T.);
#2257=ORIENTED_EDGE('',*,*,#1690,.F.);
#2258=ORIENTED_EDGE('',*,*,#1691,.T.);
#2259=ORIENTED_EDGE('',*,*,#1692,.F.);
#2260=ORIENTED_EDGE('',*,*,#1691,.F.);
#2261=ORIENTED_EDGE('',*,*,#1693,.F.);
#2262=ORIENTED_EDGE('',*,*,#1694,.T.);
#2263=ORIENTED_EDGE('',*,*,#1690,.T.);
#2264=ORIENTED_EDGE('',*,*,#1694,.F.);
#2265=ORIENTED_EDGE('',*,*,#1693,.T.);
#2266=ORIENTED_EDGE('',*,*,#1695,.F.);
#2267=ORIENTED_EDGE('',*,*,#1696,.T.);
#2268=ORIENTED_EDGE('',*,*,#1697,.F.);
#2269=ORIENTED_EDGE('',*,*,#1698,.F.);
#2270=ORIENTED_EDGE('',*,*,#1699,.F.);
#2271=ORIENTED_EDGE('',*,*,#1700,.F.);
#2272=ORIENTED_EDGE('',*,*,#1701,.F.);
#2273=ORIENTED_EDGE('',*,*,#1702,.F.);
#2274=ORIENTED_EDGE('',*,*,#1696,.F.);
#2275=ORIENTED_EDGE('',*,*,#1701,.T.);
#2276=ORIENTED_EDGE('',*,*,#1703,.F.);
#2277=ORIENTED_EDGE('',*,*,#1704,.T.);
#2278=ORIENTED_EDGE('',*,*,#1705,.T.);
#2279=ORIENTED_EDGE('',*,*,#1700,.T.);
#2280=ORIENTED_EDGE('',*,*,#1706,.F.);
#2281=ORIENTED_EDGE('',*,*,#1707,.T.);
#2282=ORIENTED_EDGE('',*,*,#1703,.T.);
#2283=ORIENTED_EDGE('',*,*,#1699,.T.);
#2284=ORIENTED_EDGE('',*,*,#1708,.F.);
#2285=ORIENTED_EDGE('',*,*,#1709,.T.);
#2286=ORIENTED_EDGE('',*,*,#1706,.T.);
#2287=ORIENTED_EDGE('',*,*,#1698,.T.);
#2288=ORIENTED_EDGE('',*,*,#1710,.F.);
#2289=ORIENTED_EDGE('',*,*,#1711,.T.);
#2290=ORIENTED_EDGE('',*,*,#1708,.T.);
#2291=ORIENTED_EDGE('',*,*,#1697,.T.);
#2292=ORIENTED_EDGE('',*,*,#1712,.F.);
#2293=ORIENTED_EDGE('',*,*,#1713,.T.);
#2294=ORIENTED_EDGE('',*,*,#1710,.T.);
#2295=ORIENTED_EDGE('',*,*,#1702,.T.);
#2296=ORIENTED_EDGE('',*,*,#1705,.F.);
#2297=ORIENTED_EDGE('',*,*,#1714,.T.);
#2298=ORIENTED_EDGE('',*,*,#1712,.T.);
#2299=ORIENTED_EDGE('',*,*,#1695,.T.);
#2300=ORIENTED_EDGE('',*,*,#1709,.F.);
#2301=ORIENTED_EDGE('',*,*,#1711,.F.);
#2302=ORIENTED_EDGE('',*,*,#1713,.F.);
#2303=ORIENTED_EDGE('',*,*,#1714,.F.);
#2304=ORIENTED_EDGE('',*,*,#1704,.F.);
#2305=ORIENTED_EDGE('',*,*,#1707,.F.);
#2306=ORIENTED_EDGE('',*,*,#1692,.T.);
#2307=ORIENTED_EDGE('',*,*,#1715,.F.);
#2308=ORIENTED_EDGE('',*,*,#1716,.F.);
#2309=ORIENTED_EDGE('',*,*,#1717,.T.);
#2310=ORIENTED_EDGE('',*,*,#1718,.F.);
#2311=ORIENTED_EDGE('',*,*,#1717,.F.);
#2312=ORIENTED_EDGE('',*,*,#1719,.F.);
#2313=ORIENTED_EDGE('',*,*,#1720,.F.);
#2314=ORIENTED_EDGE('',*,*,#1721,.F.);
#2315=ORIENTED_EDGE('',*,*,#1722,.F.);
#2316=ORIENTED_EDGE('',*,*,#1723,.F.);
#2317=ORIENTED_EDGE('',*,*,#1724,.T.);
#2318=ORIENTED_EDGE('',*,*,#1725,.F.);
#2319=ORIENTED_EDGE('',*,*,#1726,.F.);
#2320=ORIENTED_EDGE('',*,*,#1727,.F.);
#2321=ORIENTED_EDGE('',*,*,#1728,.F.);
#2322=ORIENTED_EDGE('',*,*,#1729,.F.);
#2323=ORIENTED_EDGE('',*,*,#1730,.F.);
#2324=ORIENTED_EDGE('',*,*,#1724,.F.);
#2325=ORIENTED_EDGE('',*,*,#1720,.T.);
#2326=ORIENTED_EDGE('',*,*,#1731,.T.);
#2327=ORIENTED_EDGE('',*,*,#1729,.T.);
#2328=ORIENTED_EDGE('',*,*,#1732,.F.);
#2329=ORIENTED_EDGE('',*,*,#1719,.T.);
#2330=ORIENTED_EDGE('',*,*,#1733,.T.);
#2331=ORIENTED_EDGE('',*,*,#1730,.T.);
#2332=ORIENTED_EDGE('',*,*,#1731,.F.);
#2333=ORIENTED_EDGE('',*,*,#1716,.T.);
#2334=ORIENTED_EDGE('',*,*,#1734,.T.);
#2335=ORIENTED_EDGE('',*,*,#1725,.T.);
#2336=ORIENTED_EDGE('',*,*,#1733,.F.);
#2337=ORIENTED_EDGE('',*,*,#1735,.F.);
#2338=ORIENTED_EDGE('',*,*,#1736,.T.);
#2339=ORIENTED_EDGE('',*,*,#1737,.T.);
#2340=ORIENTED_EDGE('',*,*,#1736,.F.);
#2341=ORIENTED_EDGE('',*,*,#1715,.T.);
#2342=ORIENTED_EDGE('',*,*,#1738,.T.);
#2343=ORIENTED_EDGE('',*,*,#1726,.T.);
#2344=ORIENTED_EDGE('',*,*,#1734,.F.);
#2345=ORIENTED_EDGE('',*,*,#1721,.T.);
#2346=ORIENTED_EDGE('',*,*,#1732,.T.);
#2347=ORIENTED_EDGE('',*,*,#1728,.T.);
#2348=ORIENTED_EDGE('',*,*,#1739,.F.);
#2349=ORIENTED_EDGE('',*,*,#1722,.T.);
#2350=ORIENTED_EDGE('',*,*,#1739,.T.);
#2351=ORIENTED_EDGE('',*,*,#1727,.T.);
#2352=ORIENTED_EDGE('',*,*,#1738,.F.);
#2353=ORIENTED_EDGE('',*,*,#1723,.T.);
#2354=ORIENTED_EDGE('',*,*,#1735,.T.);
#2355=ORIENTED_EDGE('',*,*,#1718,.T.);
#2356=ORIENTED_EDGE('',*,*,#1737,.F.);
#2357=ORIENTED_EDGE('',*,*,#1740,.F.);
#2358=ORIENTED_EDGE('',*,*,#1741,.T.);
#2359=ORIENTED_EDGE('',*,*,#1742,.T.);
#2360=ORIENTED_EDGE('',*,*,#1741,.F.);
#2361=ORIENTED_EDGE('',*,*,#1740,.T.);
#2362=ORIENTED_EDGE('',*,*,#1742,.F.);
#2363=ORIENTED_EDGE('',*,*,#1743,.F.);
#2364=ORIENTED_EDGE('',*,*,#1744,.T.);
#2365=ORIENTED_EDGE('',*,*,#1745,.F.);
#2366=ORIENTED_EDGE('',*,*,#1744,.F.);
#2367=ORIENTED_EDGE('',*,*,#1746,.F.);
#2368=ORIENTED_EDGE('',*,*,#1747,.F.);
#2369=ORIENTED_EDGE('',*,*,#1748,.F.);
#2370=ORIENTED_EDGE('',*,*,#1749,.F.);
#2371=ORIENTED_EDGE('',*,*,#1750,.T.);
#2372=ORIENTED_EDGE('',*,*,#1748,.T.);
#2373=ORIENTED_EDGE('',*,*,#1750,.F.);
#2374=ORIENTED_EDGE('',*,*,#1751,.F.);
#2375=ORIENTED_EDGE('',*,*,#1752,.T.);
#2376=ORIENTED_EDGE('',*,*,#1749,.T.);
#2377=ORIENTED_EDGE('',*,*,#1752,.F.);
#2378=ORIENTED_EDGE('',*,*,#1751,.T.);
#2379=ORIENTED_EDGE('',*,*,#1753,.F.);
#2380=ORIENTED_EDGE('',*,*,#1754,.F.);
#2381=ORIENTED_EDGE('',*,*,#1755,.T.);
#2382=ORIENTED_EDGE('',*,*,#1747,.T.);
#2383=ORIENTED_EDGE('',*,*,#1756,.T.);
#2384=ORIENTED_EDGE('',*,*,#1753,.T.);
#2385=ORIENTED_EDGE('',*,*,#1756,.F.);
#2386=ORIENTED_EDGE('',*,*,#1746,.T.);
#2387=ORIENTED_EDGE('',*,*,#1743,.T.);
#2388=ORIENTED_EDGE('',*,*,#1755,.F.);
#2389=ORIENTED_EDGE('',*,*,#1745,.T.);
#2390=ORIENTED_EDGE('',*,*,#1757,.F.);
#2391=ORIENTED_EDGE('',*,*,#1758,.T.);
#2392=ORIENTED_EDGE('',*,*,#1754,.T.);
#2393=ORIENTED_EDGE('',*,*,#1758,.F.);
#2394=ORIENTED_EDGE('',*,*,#1757,.T.);
#2395=ORIENTED_EDGE('',*,*,#1759,.F.);
#2396=ORIENTED_EDGE('',*,*,#1760,.T.);
#2397=ORIENTED_EDGE('',*,*,#1761,.T.);
#2398=ORIENTED_EDGE('',*,*,#1760,.F.);
#2399=ORIENTED_EDGE('',*,*,#1762,.F.);
#2400=ORIENTED_EDGE('',*,*,#1763,.T.);
#2401=ORIENTED_EDGE('',*,*,#1764,.T.);
#2402=ORIENTED_EDGE('',*,*,#1763,.F.);
#2403=ORIENTED_EDGE('',*,*,#1762,.T.);
#2404=ORIENTED_EDGE('',*,*,#1759,.T.);
#2405=ORIENTED_EDGE('',*,*,#1764,.F.);
#2406=ORIENTED_EDGE('',*,*,#1761,.F.);
#2407=ORIENTED_EDGE('',*,*,#1765,.F.);
#2408=ORIENTED_EDGE('',*,*,#1766,.T.);
#2409=ORIENTED_EDGE('',*,*,#1767,.T.);
#2410=ORIENTED_EDGE('',*,*,#1766,.F.);
#2411=ORIENTED_EDGE('',*,*,#1768,.F.);
#2412=ORIENTED_EDGE('',*,*,#1769,.T.);
#2413=ORIENTED_EDGE('',*,*,#1770,.T.);
#2414=ORIENTED_EDGE('',*,*,#1769,.F.);
#2415=ORIENTED_EDGE('',*,*,#1768,.T.);
#2416=ORIENTED_EDGE('',*,*,#1765,.T.);
#2417=ORIENTED_EDGE('',*,*,#1770,.F.);
#2418=ORIENTED_EDGE('',*,*,#1767,.F.);
#2419=ORIENTED_EDGE('',*,*,#1771,.F.);
#2420=ORIENTED_EDGE('',*,*,#1772,.T.);
#2421=ORIENTED_EDGE('',*,*,#1771,.T.);
#2422=ORIENTED_EDGE('',*,*,#1772,.F.);
#2423=ORIENTED_EDGE('',*,*,#1773,.F.);
#2424=ORIENTED_EDGE('',*,*,#1774,.F.);
#2425=ORIENTED_EDGE('',*,*,#1775,.T.);
#2426=ORIENTED_EDGE('',*,*,#1776,.F.);
#2427=ORIENTED_EDGE('',*,*,#1776,.T.);
#2428=ORIENTED_EDGE('',*,*,#1777,.T.);
#2429=ORIENTED_EDGE('',*,*,#1778,.F.);
#2430=ORIENTED_EDGE('',*,*,#1779,.F.);
#2431=ORIENTED_EDGE('',*,*,#1775,.F.);
#2432=ORIENTED_EDGE('',*,*,#1779,.T.);
#2433=ORIENTED_EDGE('',*,*,#1780,.F.);
#2434=ORIENTED_EDGE('',*,*,#1781,.T.);
#2435=ORIENTED_EDGE('',*,*,#1774,.T.);
#2436=ORIENTED_EDGE('',*,*,#1773,.T.);
#2437=ORIENTED_EDGE('',*,*,#1781,.F.);
#2438=ORIENTED_EDGE('',*,*,#1782,.F.);
#2439=ORIENTED_EDGE('',*,*,#1777,.F.);
#2440=ORIENTED_EDGE('',*,*,#1782,.T.);
#2441=ORIENTED_EDGE('',*,*,#1780,.T.);
#2442=ORIENTED_EDGE('',*,*,#1778,.T.);
#2443=CYLINDRICAL_SURFACE('',#2790,0.3);
#2444=CYLINDRICAL_SURFACE('',#2805,0.275);
#2445=CYLINDRICAL_SURFACE('',#2807,0.275);
#2446=CYLINDRICAL_SURFACE('',#2809,0.51);
#2447=CYLINDRICAL_SURFACE('',#2817,0.31);
#2448=CYLINDRICAL_SURFACE('',#2820,0.31);
#2449=CYLINDRICAL_SURFACE('',#2839,0.275);
#2450=CYLINDRICAL_SURFACE('',#2842,0.31);
#2451=CYLINDRICAL_SURFACE('',#2845,0.7);
#2452=CYLINDRICAL_SURFACE('',#2854,0.31);
#2453=CYLINDRICAL_SURFACE('',#2857,0.31);
#2454=CYLINDRICAL_SURFACE('',#2870,0.6);
#2455=CYLINDRICAL_SURFACE('',#2882,0.21);
#2456=CYLINDRICAL_SURFACE('',#2886,0.7);
#2457=CYLINDRICAL_SURFACE('',#2906,0.425);
#2458=CYLINDRICAL_SURFACE('',#2914,0.24505);
#2459=CYLINDRICAL_SURFACE('',#2917,0.31);
#2460=CYLINDRICAL_SURFACE('',#2920,0.31);
#2461=CYLINDRICAL_SURFACE('',#2923,0.6);
#2462=CYLINDRICAL_SURFACE('',#2930,0.6);
#2463=CYLINDRICAL_SURFACE('',#2936,0.34);
#2464=CYLINDRICAL_SURFACE('',#2940,0.31);
#2465=CYLINDRICAL_SURFACE('',#2943,0.31);
#2466=CYLINDRICAL_SURFACE('',#2957,0.5);
#2467=CYLINDRICAL_SURFACE('',#2961,0.3933);
#2468=CYLINDRICAL_SURFACE('',#2985,0.338975);
#2469=CYLINDRICAL_SURFACE('',#2994,1.);
#2470=CYLINDRICAL_SURFACE('',#3000,0.08);
#2471=CYLINDRICAL_SURFACE('',#3005,0.5);
#2472=CYLINDRICAL_SURFACE('',#3009,0.3);
#2473=CYLINDRICAL_SURFACE('',#3015,0.32);
#2474=CYLINDRICAL_SURFACE('',#3018,0.6);
#2475=CYLINDRICAL_SURFACE('',#3024,0.31);
#2476=CYLINDRICAL_SURFACE('',#3027,0.5);
#2477=CYLINDRICAL_SURFACE('',#3039,0.08);
#2478=ADVANCED_FACE('',(#362),#2443,.T.);
#2479=ADVANCED_FACE('',(#363),#256,.F.);
#2480=ADVANCED_FACE('',(#364),#257,.T.);
#2481=ADVANCED_FACE('',(#365),#258,.T.);
#2482=ADVANCED_FACE('',(#366),#259,.T.);
#2483=ADVANCED_FACE('',(#367),#260,.T.);
#2484=ADVANCED_FACE('',(#368),#261,.T.);
#2485=ADVANCED_FACE('',(#369),#262,.F.);
#2486=ADVANCED_FACE('',(#370,#210,#211,#212,#213,#214),#263,.T.);
#2487=ADVANCED_FACE('',(#371),#2444,.F.);
#2488=ADVANCED_FACE('',(#372),#2445,.F.);
#2489=ADVANCED_FACE('',(#373),#2446,.F.);
#2490=ADVANCED_FACE('',(#374),#264,.F.);
#2491=ADVANCED_FACE('',(#375,#215),#265,.T.);
#2492=ADVANCED_FACE('',(#376,#216),#266,.T.);
#2493=ADVANCED_FACE('',(#377),#267,.T.);
#2494=ADVANCED_FACE('',(#378),#268,.T.);
#2495=ADVANCED_FACE('',(#379),#2447,.F.);
#2496=ADVANCED_FACE('',(#380),#2448,.F.);
#2497=ADVANCED_FACE('',(#381,#217),#269,.F.);
#2498=ADVANCED_FACE('',(#382),#270,.T.);
#2499=ADVANCED_FACE('',(#383),#271,.T.);
#2500=ADVANCED_FACE('',(#384),#272,.T.);
#2501=ADVANCED_FACE('',(#385,#218),#273,.T.);
#2502=ADVANCED_FACE('',(#386,#219),#274,.F.);
#2503=ADVANCED_FACE('',(#387),#275,.T.);
#2504=ADVANCED_FACE('',(#388),#276,.T.);
#2505=ADVANCED_FACE('',(#389),#277,.T.);
#2506=ADVANCED_FACE('',(#390,#220),#278,.T.);
#2507=ADVANCED_FACE('',(#391),#279,.T.);
#2508=ADVANCED_FACE('',(#392),#280,.T.);
#2509=ADVANCED_FACE('',(#393),#281,.T.);
#2510=ADVANCED_FACE('',(#394,#221,#222),#282,.F.);
#2511=ADVANCED_FACE('',(#395),#2449,.F.);
#2512=ADVANCED_FACE('',(#396),#2450,.F.);
#2513=ADVANCED_FACE('',(#397),#2451,.T.);
#2514=ADVANCED_FACE('',(#398,#223),#283,.F.);
#2515=ADVANCED_FACE('',(#399),#284,.T.);
#2516=ADVANCED_FACE('',(#400,#224),#285,.T.);
#2517=ADVANCED_FACE('',(#401),#286,.T.);
#2518=ADVANCED_FACE('',(#402),#2452,.F.);
#2519=ADVANCED_FACE('',(#403),#2453,.F.);
#2520=ADVANCED_FACE('',(#404),#287,.T.);
#2521=ADVANCED_FACE('',(#405,#225),#288,.T.);
#2522=ADVANCED_FACE('',(#406),#289,.T.);
#2523=ADVANCED_FACE('',(#407,#226),#290,.F.);
#2524=ADVANCED_FACE('',(#408),#291,.F.);
#2525=ADVANCED_FACE('',(#409),#292,.T.);
#2526=ADVANCED_FACE('',(#410),#293,.T.);
#2527=ADVANCED_FACE('',(#411),#294,.T.);
#2528=ADVANCED_FACE('',(#412,#227,#228),#2454,.T.);
#2529=ADVANCED_FACE('',(#413,#229),#295,.T.);
#2530=ADVANCED_FACE('',(#414,#230),#296,.F.);
#2531=ADVANCED_FACE('',(#415),#297,.T.);
#2532=ADVANCED_FACE('',(#416,#231),#298,.T.);
#2533=ADVANCED_FACE('',(#417,#232),#299,.T.);
#2534=ADVANCED_FACE('',(#418),#300,.T.);
#2535=ADVANCED_FACE('',(#419),#301,.T.);
#2536=ADVANCED_FACE('',(#420,#233),#302,.F.);
#2537=ADVANCED_FACE('',(#421),#2455,.F.);
#2538=ADVANCED_FACE('',(#422),#303,.T.);
#2539=ADVANCED_FACE('',(#423),#2456,.T.);
#2540=ADVANCED_FACE('',(#424,#234),#304,.T.);
#2541=ADVANCED_FACE('',(#425),#305,.F.);
#2542=ADVANCED_FACE('',(#426),#306,.F.);
#2543=ADVANCED_FACE('',(#427),#307,.F.);
#2544=ADVANCED_FACE('',(#428),#308,.F.);
#2545=ADVANCED_FACE('',(#429),#309,.F.);
#2546=ADVANCED_FACE('',(#430),#310,.F.);
#2547=ADVANCED_FACE('',(#431),#311,.F.);
#2548=ADVANCED_FACE('',(#432),#312,.F.);
#2549=ADVANCED_FACE('',(#433),#313,.F.);
#2550=ADVANCED_FACE('',(#434),#314,.F.);
#2551=ADVANCED_FACE('',(#435),#315,.T.);
#2552=ADVANCED_FACE('',(#436),#148,.T.);
#2553=ADVANCED_FACE('',(#437),#2457,.T.);
#2554=ADVANCED_FACE('',(#438),#149,.T.);
#2555=ADVANCED_FACE('',(#439,#235),#316,.T.);
#2556=ADVANCED_FACE('',(#440),#150,.T.);
#2557=ADVANCED_FACE('',(#441),#2458,.T.);
#2558=ADVANCED_FACE('',(#442),#2459,.F.);
#2559=ADVANCED_FACE('',(#443),#2460,.F.);
#2560=ADVANCED_FACE('',(#444),#2461,.T.);
#2561=ADVANCED_FACE('',(#445),#317,.T.);
#2562=ADVANCED_FACE('',(#446,#236,#237),#318,.F.);
#2563=ADVANCED_FACE('',(#447),#319,.T.);
#2564=ADVANCED_FACE('',(#448),#2462,.T.);
#2565=ADVANCED_FACE('',(#449,#238,#239),#320,.T.);
#2566=ADVANCED_FACE('',(#450),#2463,.F.);
#2567=ADVANCED_FACE('',(#451),#321,.T.);
#2568=ADVANCED_FACE('',(#452),#2464,.F.);
#2569=ADVANCED_FACE('',(#453),#2465,.F.);
#2570=ADVANCED_FACE('',(#454),#322,.T.);
#2571=ADVANCED_FACE('',(#455,#240),#323,.T.);
#2572=ADVANCED_FACE('',(#456),#324,.T.);
#2573=ADVANCED_FACE('',(#457,#241),#325,.F.);
#2574=ADVANCED_FACE('',(#458),#326,.T.);
#2575=ADVANCED_FACE('',(#459,#242),#327,.T.);
#2576=ADVANCED_FACE('',(#460),#328,.T.);
#2577=ADVANCED_FACE('',(#461,#243),#329,.F.);
#2578=ADVANCED_FACE('',(#462),#330,.T.);
#2579=ADVANCED_FACE('',(#463,#244),#331,.T.);
#2580=ADVANCED_FACE('',(#464),#2466,.T.);
#2581=ADVANCED_FACE('',(#465,#245),#332,.T.);
#2582=ADVANCED_FACE('',(#466),#2467,.T.);
#2583=ADVANCED_FACE('',(#467),#151,.T.);
#2584=ADVANCED_FACE('',(#468),#333,.T.);
#2585=ADVANCED_FACE('',(#469),#152,.T.);
#2586=ADVANCED_FACE('',(#470),#334,.T.);
#2587=ADVANCED_FACE('',(#471),#335,.T.);
#2588=ADVANCED_FACE('',(#472),#336,.T.);
#2589=ADVANCED_FACE('',(#473),#337,.T.);
#2590=ADVANCED_FACE('',(#474),#338,.T.);
#2591=ADVANCED_FACE('',(#475),#339,.T.);
#2592=ADVANCED_FACE('',(#476),#340,.T.);
#2593=ADVANCED_FACE('',(#477,#246),#341,.F.);
#2594=ADVANCED_FACE('',(#478),#153,.T.);
#2595=ADVANCED_FACE('',(#479),#154,.T.);
#2596=ADVANCED_FACE('',(#480),#342,.T.);
#2597=ADVANCED_FACE('',(#481),#343,.T.);
#2598=ADVANCED_FACE('',(#482),#344,.T.);
#2599=ADVANCED_FACE('',(#483),#2468,.F.);
#2600=ADVANCED_FACE('',(#484),#345,.T.);
#2601=ADVANCED_FACE('',(#485),#346,.T.);
#2602=ADVANCED_FACE('',(#486),#347,.T.);
#2603=ADVANCED_FACE('',(#487,#247),#348,.T.);
#2604=ADVANCED_FACE('',(#488,#248),#349,.F.);
#2605=ADVANCED_FACE('',(#489),#2469,.T.);
#2606=ADVANCED_FACE('',(#490),#350,.T.);
#2607=ADVANCED_FACE('',(#491),#351,.F.);
#2608=ADVANCED_FACE('',(#492),#2470,.F.);
#2609=ADVANCED_FACE('',(#493),#352,.T.);
#2610=ADVANCED_FACE('',(#494),#155,.T.);
#2611=ADVANCED_FACE('',(#495),#2471,.T.);
#2612=ADVANCED_FACE('',(#496,#249),#353,.T.);
#2613=ADVANCED_FACE('',(#497,#250),#2472,.T.);
#2614=ADVANCED_FACE('',(#498),#156,.T.);
#2615=ADVANCED_FACE('',(#499),#354,.T.);
#2616=ADVANCED_FACE('',(#500),#2473,.F.);
#2617=ADVANCED_FACE('',(#501),#2474,.T.);
#2618=ADVANCED_FACE('',(#502,#251),#355,.T.);
#2619=ADVANCED_FACE('',(#503,#252),#356,.F.);
#2620=ADVANCED_FACE('',(#504),#2475,.F.);
#2621=ADVANCED_FACE('',(#505),#2476,.T.);
#2622=ADVANCED_FACE('',(#506,#253),#357,.T.);
#2623=ADVANCED_FACE('',(#507,#254),#358,.F.);
#2624=ADVANCED_FACE('',(#508,#255),#11,.T.);
#2625=ADVANCED_FACE('',(#509),#359,.F.);
#2626=ADVANCED_FACE('',(#510),#360,.T.);
#2627=ADVANCED_FACE('',(#511),#2477,.T.);
#2628=ADVANCED_FACE('',(#512),#361,.F.);
#2629=CLOSED_SHELL('',(#2478,#2479,#2480,#2481,#2482,#2483,#2484,#2485,
#2486,#2487,#2488,#2489,#2490,#2491,#2492,#2493,#2494,#2495,#2496,#2497,
#2498,#2499,#2500,#2501,#2502,#2503,#2504,#2505,#2506,#2507,#2508,#2509,
#2510));
#2630=CLOSED_SHELL('',(#2511,#2512,#2513,#2514,#2515,#2516,#2517,#2518,
#2519,#2520,#2521,#2522,#2523,#2524,#2525,#2526,#2527,#2528,#2529,#2530,
#2531,#2532,#2533,#2534,#2535,#2536));
#2631=CLOSED_SHELL('',(#2537,#2538,#2539,#2540,#2541));
#2632=CLOSED_SHELL('',(#2542,#2543,#2544,#2545,#2546,#2547,#2548,#2549));
#2633=CLOSED_SHELL('',(#2550,#2551,#2552,#2553,#2554,#2555,#2556,#2557));
#2634=CLOSED_SHELL('',(#2558,#2559,#2560,#2561,#2562,#2563,#2564,#2565));
#2635=CLOSED_SHELL('',(#2566,#2567,#2568,#2569,#2570,#2571,#2572,#2573,
#2574,#2575,#2576,#2577,#2578,#2579,#2580,#2581));
#2636=CLOSED_SHELL('',(#2582,#2583,#2584,#2585,#2586,#2587,#2588,#2589,
#2590,#2591,#2592,#2593));
#2637=CLOSED_SHELL('',(#2594,#2595,#2596,#2597,#2598,#2599,#2600,#2601,
#2602,#2603,#2604));
#2638=CLOSED_SHELL('',(#2605,#2606,#2607));
#2639=CLOSED_SHELL('',(#2608,#2609,#2610,#2611,#2612,#2613,#2614,#2615));
#2640=CLOSED_SHELL('',(#2616,#2617,#2618,#2619));
#2641=CLOSED_SHELL('',(#2620,#2621,#2622,#2623));
#2642=CLOSED_SHELL('',(#2624,#2625,#2626,#2627,#2628));
#2643=DERIVED_UNIT_ELEMENT(#2669,1.);
#2644=DERIVED_UNIT_ELEMENT(#4793,-3.);
#2645=DERIVED_UNIT_ELEMENT(#2669,1.);
#2646=DERIVED_UNIT_ELEMENT(#4793,-3.);
#2647=DERIVED_UNIT_ELEMENT(#2669,1.);
#2648=DERIVED_UNIT_ELEMENT(#4793,-3.);
#2649=DERIVED_UNIT_ELEMENT(#2669,1.);
#2650=DERIVED_UNIT_ELEMENT(#4793,-3.);
#2651=DERIVED_UNIT_ELEMENT(#2669,1.);
#2652=DERIVED_UNIT_ELEMENT(#4793,-3.);
#2653=DERIVED_UNIT_ELEMENT(#2669,1.);
#2654=DERIVED_UNIT_ELEMENT(#4793,-3.);
#2655=DERIVED_UNIT_ELEMENT(#2669,1.);
#2656=DERIVED_UNIT_ELEMENT(#4793,-3.);
#2657=DERIVED_UNIT_ELEMENT(#2669,1.);
#2658=DERIVED_UNIT_ELEMENT(#4793,-3.);
#2659=DERIVED_UNIT_ELEMENT(#2669,1.);
#2660=DERIVED_UNIT_ELEMENT(#4793,-3.);
#2661=DERIVED_UNIT_ELEMENT(#2669,1.);
#2662=DERIVED_UNIT_ELEMENT(#4793,-3.);
#2663=DERIVED_UNIT_ELEMENT(#2669,1.);
#2664=DERIVED_UNIT_ELEMENT(#4793,-3.);
#2665=DERIVED_UNIT_ELEMENT(#2669,1.);
#2666=DERIVED_UNIT_ELEMENT(#4793,-3.);
#2667=DERIVED_UNIT_ELEMENT(#2669,1.);
#2668=DERIVED_UNIT_ELEMENT(#4793,-3.);
#2669=(
MASS_UNIT()
NAMED_UNIT(*)
SI_UNIT(.KILO.,.GRAM.)
);
#2670=DERIVED_UNIT((#2643,#2644));
#2671=DERIVED_UNIT((#2645,#2646));
#2672=DERIVED_UNIT((#2647,#2648));
#2673=DERIVED_UNIT((#2649,#2650));
#2674=DERIVED_UNIT((#2651,#2652));
#2675=DERIVED_UNIT((#2653,#2654));
#2676=DERIVED_UNIT((#2655,#2656));
#2677=DERIVED_UNIT((#2657,#2658));
#2678=DERIVED_UNIT((#2659,#2660));
#2679=DERIVED_UNIT((#2661,#2662));
#2680=DERIVED_UNIT((#2663,#2664));
#2681=DERIVED_UNIT((#2665,#2666));
#2682=DERIVED_UNIT((#2667,#2668));
#2683=MEASURE_REPRESENTATION_ITEM('density measure',
POSITIVE_RATIO_MEASURE(7850.),#2670);
#2684=MEASURE_REPRESENTATION_ITEM('density measure',
POSITIVE_RATIO_MEASURE(7850.),#2671);
#2685=MEASURE_REPRESENTATION_ITEM('density measure',
POSITIVE_RATIO_MEASURE(7850.),#2672);
#2686=MEASURE_REPRESENTATION_ITEM('density measure',
POSITIVE_RATIO_MEASURE(7850.),#2673);
#2687=MEASURE_REPRESENTATION_ITEM('density measure',
POSITIVE_RATIO_MEASURE(7850.),#2674);
#2688=MEASURE_REPRESENTATION_ITEM('density measure',
POSITIVE_RATIO_MEASURE(7850.),#2675);
#2689=MEASURE_REPRESENTATION_ITEM('density measure',
POSITIVE_RATIO_MEASURE(7850.),#2676);
#2690=MEASURE_REPRESENTATION_ITEM('density measure',
POSITIVE_RATIO_MEASURE(7850.),#2677);
#2691=MEASURE_REPRESENTATION_ITEM('density measure',
POSITIVE_RATIO_MEASURE(7850.),#2678);
#2692=MEASURE_REPRESENTATION_ITEM('density measure',
POSITIVE_RATIO_MEASURE(7850.),#2679);
#2693=MEASURE_REPRESENTATION_ITEM('density measure',
POSITIVE_RATIO_MEASURE(7850.),#2680);
#2694=MEASURE_REPRESENTATION_ITEM('density measure',
POSITIVE_RATIO_MEASURE(7850.),#2681);
#2695=MEASURE_REPRESENTATION_ITEM('density measure',
POSITIVE_RATIO_MEASURE(7850.),#2682);
#2696=PROPERTY_DEFINITION_REPRESENTATION(#2761,#2722);
#2697=PROPERTY_DEFINITION_REPRESENTATION(#2762,#2723);
#2698=PROPERTY_DEFINITION_REPRESENTATION(#2763,#2724);
#2699=PROPERTY_DEFINITION_REPRESENTATION(#2764,#2725);
#2700=PROPERTY_DEFINITION_REPRESENTATION(#2765,#2726);
#2701=PROPERTY_DEFINITION_REPRESENTATION(#2766,#2727);
#2702=PROPERTY_DEFINITION_REPRESENTATION(#2767,#2728);
#2703=PROPERTY_DEFINITION_REPRESENTATION(#2768,#2729);
#2704=PROPERTY_DEFINITION_REPRESENTATION(#2769,#2730);
#2705=PROPERTY_DEFINITION_REPRESENTATION(#2770,#2731);
#2706=PROPERTY_DEFINITION_REPRESENTATION(#2771,#2732);
#2707=PROPERTY_DEFINITION_REPRESENTATION(#2772,#2733);
#2708=PROPERTY_DEFINITION_REPRESENTATION(#2773,#2734);
#2709=PROPERTY_DEFINITION_REPRESENTATION(#2774,#2735);
#2710=PROPERTY_DEFINITION_REPRESENTATION(#2775,#2736);
#2711=PROPERTY_DEFINITION_REPRESENTATION(#2776,#2737);
#2712=PROPERTY_DEFINITION_REPRESENTATION(#2777,#2738);
#2713=PROPERTY_DEFINITION_REPRESENTATION(#2778,#2739);
#2714=PROPERTY_DEFINITION_REPRESENTATION(#2779,#2740);
#2715=PROPERTY_DEFINITION_REPRESENTATION(#2780,#2741);
#2716=PROPERTY_DEFINITION_REPRESENTATION(#2781,#2742);
#2717=PROPERTY_DEFINITION_REPRESENTATION(#2782,#2743);
#2718=PROPERTY_DEFINITION_REPRESENTATION(#2783,#2744);
#2719=PROPERTY_DEFINITION_REPRESENTATION(#2784,#2745);
#2720=PROPERTY_DEFINITION_REPRESENTATION(#2785,#2746);
#2721=PROPERTY_DEFINITION_REPRESENTATION(#2786,#2747);
#2722=REPRESENTATION('material name',(#2748),#4775);
#2723=REPRESENTATION('density',(#2683),#4775);
#2724=REPRESENTATION('material name',(#2749),#4777);
#2725=REPRESENTATION('density',(#2684),#4777);
#2726=REPRESENTATION('material name',(#2750),#4778);
#2727=REPRESENTATION('density',(#2685),#4778);
#2728=REPRESENTATION('material name',(#2751),#4779);
#2729=REPRESENTATION('density',(#2686),#4779);
#2730=REPRESENTATION('material name',(#2752),#4781);
#2731=REPRESENTATION('density',(#2687),#4781);
#2732=REPRESENTATION('material name',(#2753),#4783);
#2733=REPRESENTATION('density',(#2688),#4783);
#2734=REPRESENTATION('material name',(#2754),#4784);
#2735=REPRESENTATION('density',(#2689),#4784);
#2736=REPRESENTATION('material name',(#2755),#4785);
#2737=REPRESENTATION('density',(#2690),#4785);
#2738=REPRESENTATION('material name',(#2756),#4786);
#2739=REPRESENTATION('density',(#2691),#4786);
#2740=REPRESENTATION('material name',(#2757),#4787);
#2741=REPRESENTATION('density',(#2692),#4787);
#2742=REPRESENTATION('material name',(#2758),#4788);
#2743=REPRESENTATION('density',(#2693),#4788);
#2744=REPRESENTATION('material name',(#2759),#4789);
#2745=REPRESENTATION('density',(#2694),#4789);
#2746=REPRESENTATION('material name',(#2760),#4790);
#2747=REPRESENTATION('density',(#2695),#4790);
#2748=DESCRIPTIVE_REPRESENTATION_ITEM('Steel','Steel');
#2749=DESCRIPTIVE_REPRESENTATION_ITEM('Steel','Steel');
#2750=DESCRIPTIVE_REPRESENTATION_ITEM('Steel','Steel');
#2751=DESCRIPTIVE_REPRESENTATION_ITEM('Steel','Steel');
#2752=DESCRIPTIVE_REPRESENTATION_ITEM('Steel','Steel');
#2753=DESCRIPTIVE_REPRESENTATION_ITEM('Steel','Steel');
#2754=DESCRIPTIVE_REPRESENTATION_ITEM('Steel','Steel');
#2755=DESCRIPTIVE_REPRESENTATION_ITEM('Steel','Steel');
#2756=DESCRIPTIVE_REPRESENTATION_ITEM('Steel','Steel');
#2757=DESCRIPTIVE_REPRESENTATION_ITEM('Steel','Steel');
#2758=DESCRIPTIVE_REPRESENTATION_ITEM('Steel','Steel');
#2759=DESCRIPTIVE_REPRESENTATION_ITEM('Steel','Steel');
#2760=DESCRIPTIVE_REPRESENTATION_ITEM('Steel','Steel');
#2761=PROPERTY_DEFINITION('material property','material name',#4881);
#2762=PROPERTY_DEFINITION('material property','density of part',#4881);
#2763=PROPERTY_DEFINITION('material property','material name',#4883);
#2764=PROPERTY_DEFINITION('material property','density of part',#4883);
#2765=PROPERTY_DEFINITION('material property','material name',#4884);
#2766=PROPERTY_DEFINITION('material property','density of part',#4884);
#2767=PROPERTY_DEFINITION('material property','material name',#4885);
#2768=PROPERTY_DEFINITION('material property','density of part',#4885);
#2769=PROPERTY_DEFINITION('material property','material name',#4887);
#2770=PROPERTY_DEFINITION('material property','density of part',#4887);
#2771=PROPERTY_DEFINITION('material property','material name',#4889);
#2772=PROPERTY_DEFINITION('material property','density of part',#4889);
#2773=PROPERTY_DEFINITION('material property','material name',#4890);
#2774=PROPERTY_DEFINITION('material property','density of part',#4890);
#2775=PROPERTY_DEFINITION('material property','material name',#4891);
#2776=PROPERTY_DEFINITION('material property','density of part',#4891);
#2777=PROPERTY_DEFINITION('material property','material name',#4892);
#2778=PROPERTY_DEFINITION('material property','density of part',#4892);
#2779=PROPERTY_DEFINITION('material property','material name',#4893);
#2780=PROPERTY_DEFINITION('material property','density of part',#4893);
#2781=PROPERTY_DEFINITION('material property','material name',#4894);
#2782=PROPERTY_DEFINITION('material property','density of part',#4894);
#2783=PROPERTY_DEFINITION('material property','material name',#4895);
#2784=PROPERTY_DEFINITION('material property','density of part',#4895);
#2785=PROPERTY_DEFINITION('material property','material name',#4896);
#2786=PROPERTY_DEFINITION('material property','density of part',#4896);
#2787=AXIS2_PLACEMENT_3D('',#3856,#3070,#3071);
#2788=AXIS2_PLACEMENT_3D('',#3857,#3072,#3073);
#2789=AXIS2_PLACEMENT_3D('',#3858,#3074,#3075);
#2790=AXIS2_PLACEMENT_3D('',#3859,#3076,#3077);
#2791=AXIS2_PLACEMENT_3D('',#3864,#3079,#3080);
#2792=AXIS2_PLACEMENT_3D('',#3868,#3082,#3083);
#2793=AXIS2_PLACEMENT_3D('',#3871,#3085,#3086);
#2794=AXIS2_PLACEMENT_3D('',#3872,#3087,#3088);
#2795=AXIS2_PLACEMENT_3D('',#3873,#3089,#3090);
#2796=AXIS2_PLACEMENT_3D('',#3874,#3091,#3092);
#2797=AXIS2_PLACEMENT_3D('',#3892,#3102,#3103);
#2798=AXIS2_PLACEMENT_3D('',#3896,#3106,#3107);
#2799=AXIS2_PLACEMENT_3D('',#3900,#3110,#3111);
#2800=AXIS2_PLACEMENT_3D('',#3904,#3114,#3115);
#2801=AXIS2_PLACEMENT_3D('',#3908,#3118,#3119);
#2802=AXIS2_PLACEMENT_3D('',#3910,#3121,#3122);
#2803=AXIS2_PLACEMENT_3D('',#3941,#3138,#3139);
#2804=AXIS2_PLACEMENT_3D('',#3943,#3140,#3141);
#2805=AXIS2_PLACEMENT_3D('',#3944,#3142,#3143);
#2806=AXIS2_PLACEMENT_3D('',#3946,#3144,#3145);
#2807=AXIS2_PLACEMENT_3D('',#3948,#3147,#3148);
#2808=AXIS2_PLACEMENT_3D('',#3950,#3149,#3150);
#2809=AXIS2_PLACEMENT_3D('',#3952,#3152,#3153);
#2810=AXIS2_PLACEMENT_3D('',#3954,#3154,#3155);
#2811=AXIS2_PLACEMENT_3D('',#3957,#3157,#3158);
#2812=AXIS2_PLACEMENT_3D('',#3958,#3159,#3160);
#2813=AXIS2_PLACEMENT_3D('',#3964,#3164,#3165);
#2814=AXIS2_PLACEMENT_3D('',#3968,#3168,#3169);
#2815=AXIS2_PLACEMENT_3D('',#3972,#3172,#3173);
#2816=AXIS2_PLACEMENT_3D('',#3974,#3175,#3176);
#2817=AXIS2_PLACEMENT_3D('',#3975,#3177,#3178);
#2818=AXIS2_PLACEMENT_3D('',#3977,#3179,#3180);
#2819=AXIS2_PLACEMENT_3D('',#3980,#3182,#3183);
#2820=AXIS2_PLACEMENT_3D('',#3981,#3184,#3185);
#2821=AXIS2_PLACEMENT_3D('',#3983,#3186,#3187);
#2822=AXIS2_PLACEMENT_3D('',#3986,#3189,#3190);
#2823=AXIS2_PLACEMENT_3D('',#3987,#3191,#3192);
#2824=AXIS2_PLACEMENT_3D('',#3993,#3196,#3197);
#2825=AXIS2_PLACEMENT_3D('',#3997,#3200,#3201);
#2826=AXIS2_PLACEMENT_3D('',#4001,#3204,#3205);
#2827=AXIS2_PLACEMENT_3D('',#4003,#3207,#3208);
#2828=AXIS2_PLACEMENT_3D('',#4004,#3209,#3210);
#2829=AXIS2_PLACEMENT_3D('',#4010,#3214,#3215);
#2830=AXIS2_PLACEMENT_3D('',#4014,#3218,#3219);
#2831=AXIS2_PLACEMENT_3D('',#4018,#3222,#3223);
#2832=AXIS2_PLACEMENT_3D('',#4020,#3225,#3226);
#2833=AXIS2_PLACEMENT_3D('',#4021,#3227,#3228);
#2834=AXIS2_PLACEMENT_3D('',#4025,#3231,#3232);
#2835=AXIS2_PLACEMENT_3D('',#4029,#3235,#3236);
#2836=AXIS2_PLACEMENT_3D('',#4031,#3238,#3239);
#2837=AXIS2_PLACEMENT_3D('',#4032,#3240,#3241);
#2838=AXIS2_PLACEMENT_3D('',#4033,#3242,#3243);
#2839=AXIS2_PLACEMENT_3D('',#4034,#3244,#3245);
#2840=AXIS2_PLACEMENT_3D('',#4036,#3246,#3247);
#2841=AXIS2_PLACEMENT_3D('',#4039,#3249,#3250);
#2842=AXIS2_PLACEMENT_3D('',#4040,#3251,#3252);
#2843=AXIS2_PLACEMENT_3D('',#4042,#3253,#3254);
#2844=AXIS2_PLACEMENT_3D('',#4045,#3256,#3257);
#2845=AXIS2_PLACEMENT_3D('',#4046,#3258,#3259);
#2846=AXIS2_PLACEMENT_3D('',#4051,#3261,#3262);
#2847=AXIS2_PLACEMENT_3D('',#4054,#3264,#3265);
#2848=AXIS2_PLACEMENT_3D('',#4055,#3266,#3267);
#2849=AXIS2_PLACEMENT_3D('',#4059,#3269,#3270);
#2850=AXIS2_PLACEMENT_3D('',#4061,#3272,#3273);
#2851=AXIS2_PLACEMENT_3D('',#4065,#3276,#3277);
#2852=AXIS2_PLACEMENT_3D('',#4068,#3279,#3280);
#2853=AXIS2_PLACEMENT_3D('',#4069,#3281,#3282);
#2854=AXIS2_PLACEMENT_3D('',#4071,#3284,#3285);
#2855=AXIS2_PLACEMENT_3D('',#4073,#3286,#3287);
#2856=AXIS2_PLACEMENT_3D('',#4076,#3289,#3290);
#2857=AXIS2_PLACEMENT_3D('',#4077,#3291,#3292);
#2858=AXIS2_PLACEMENT_3D('',#4079,#3293,#3294);
#2859=AXIS2_PLACEMENT_3D('',#4082,#3296,#3297);
#2860=AXIS2_PLACEMENT_3D('',#4083,#3298,#3299);
#2861=AXIS2_PLACEMENT_3D('',#4092,#3304,#3305);
#2862=AXIS2_PLACEMENT_3D('',#4101,#3310,#3311);
#2863=AXIS2_PLACEMENT_3D('',#4107,#3315,#3316);
#2864=AXIS2_PLACEMENT_3D('',#4110,#3319,#3320);
#2865=AXIS2_PLACEMENT_3D('',#4117,#3323,#3324);
#2866=AXIS2_PLACEMENT_3D('',#4119,#3326,#3327);
#2867=AXIS2_PLACEMENT_3D('',#4125,#3331,#3332);
#2868=AXIS2_PLACEMENT_3D('',#4130,#3335,#3336);
#2869=AXIS2_PLACEMENT_3D('',#4131,#3337,#3338);
#2870=AXIS2_PLACEMENT_3D('',#4134,#3341,#3342);
#2871=AXIS2_PLACEMENT_3D('',#4136,#3343,#3344);
#2872=AXIS2_PLACEMENT_3D('',#4139,#3346,#3347);
#2873=AXIS2_PLACEMENT_3D('',#4140,#3348,#3349);
#2874=AXIS2_PLACEMENT_3D('',#4141,#3350,#3351);
#2875=AXIS2_PLACEMENT_3D('',#4142,#3352,#3353);
#2876=AXIS2_PLACEMENT_3D('',#4150,#3358,#3359);
#2877=AXIS2_PLACEMENT_3D('',#4154,#3362,#3363);
#2878=AXIS2_PLACEMENT_3D('',#4158,#3366,#3367);
#2879=AXIS2_PLACEMENT_3D('',#4162,#3370,#3371);
#2880=AXIS2_PLACEMENT_3D('',#4164,#3373,#3374);
#2881=AXIS2_PLACEMENT_3D('',#4165,#3375,#3376);
#2882=AXIS2_PLACEMENT_3D('',#4166,#3377,#3378);
#2883=AXIS2_PLACEMENT_3D('',#4168,#3379,#3380);
#2884=AXIS2_PLACEMENT_3D('',#4171,#3382,#3383);
#2885=AXIS2_PLACEMENT_3D('',#4172,#3384,#3385);
#2886=AXIS2_PLACEMENT_3D('',#4173,#3386,#3387);
#2887=AXIS2_PLACEMENT_3D('',#4175,#3388,#3389);
#2888=AXIS2_PLACEMENT_3D('',#4178,#3391,#3392);
#2889=AXIS2_PLACEMENT_3D('',#4179,#3393,#3394);
#2890=AXIS2_PLACEMENT_3D('',#4180,#3395,#3396);
#2891=AXIS2_PLACEMENT_3D('',#4181,#3397,#3398);
#2892=AXIS2_PLACEMENT_3D('',#4182,#3399,#3400);
#2893=AXIS2_PLACEMENT_3D('',#4191,#3405,#3406);
#2894=AXIS2_PLACEMENT_3D('',#4197,#3410,#3411);
#2895=AXIS2_PLACEMENT_3D('',#4203,#3415,#3416);
#2896=AXIS2_PLACEMENT_3D('',#4209,#3420,#3421);
#2897=AXIS2_PLACEMENT_3D('',#4215,#3425,#3426);
#2898=AXIS2_PLACEMENT_3D('',#4218,#3429,#3430);
#2899=AXIS2_PLACEMENT_3D('',#4219,#3431,#3432);
#2900=AXIS2_PLACEMENT_3D('',#4220,#3433,#3434);
#2901=AXIS2_PLACEMENT_3D('',#4222,#3435,#3436);
#2902=AXIS2_PLACEMENT_3D('',#4223,#3437,#3438);
#2903=AXIS2_PLACEMENT_3D('',#4225,#3439,#3440);
#2904=AXIS2_PLACEMENT_3D('',#4226,#3441,#3442);
#2905=AXIS2_PLACEMENT_3D('',#4228,#3443,#3444);
#2906=AXIS2_PLACEMENT_3D('',#4230,#3446,#3447);
#2907=AXIS2_PLACEMENT_3D('',#4232,#3448,#3449);
#2908=AXIS2_PLACEMENT_3D('',#4234,#3451,#3452);
#2909=AXIS2_PLACEMENT_3D('',#4236,#3453,#3454);
#2910=AXIS2_PLACEMENT_3D('',#4238,#3456,#3457);
#2911=AXIS2_PLACEMENT_3D('',#4240,#3458,#3459);
#2912=AXIS2_PLACEMENT_3D('',#4241,#3460,#3461);
#2913=AXIS2_PLACEMENT_3D('',#4243,#3462,#3463);
#2914=AXIS2_PLACEMENT_3D('',#4245,#3465,#3466);
#2915=AXIS2_PLACEMENT_3D('',#4247,#3468,#3469);
#2916=AXIS2_PLACEMENT_3D('',#4248,#3470,#3471);
#2917=AXIS2_PLACEMENT_3D('',#4249,#3472,#3473);
#2918=AXIS2_PLACEMENT_3D('',#4251,#3474,#3475);
#2919=AXIS2_PLACEMENT_3D('',#4254,#3477,#3478);
#2920=AXIS2_PLACEMENT_3D('',#4255,#3479,#3480);
#2921=AXIS2_PLACEMENT_3D('',#4257,#3481,#3482);
#2922=AXIS2_PLACEMENT_3D('',#4260,#3484,#3485);
#2923=AXIS2_PLACEMENT_3D('',#4261,#3486,#3487);
#2924=AXIS2_PLACEMENT_3D('',#4266,#3489,#3490);
#2925=AXIS2_PLACEMENT_3D('',#4269,#3492,#3493);
#2926=AXIS2_PLACEMENT_3D('',#4270,#3494,#3495);
#2927=AXIS2_PLACEMENT_3D('',#4276,#3499,#3500);
#2928=AXIS2_PLACEMENT_3D('',#4279,#3502,#3503);
#2929=AXIS2_PLACEMENT_3D('',#4280,#3504,#3505);
#2930=AXIS2_PLACEMENT_3D('',#4284,#3508,#3509);
#2931=AXIS2_PLACEMENT_3D('',#4285,#3510,#3511);
#2932=AXIS2_PLACEMENT_3D('',#4286,#3512,#3513);
#2933=AXIS2_PLACEMENT_3D('',#4287,#3514,#3515);
#2934=AXIS2_PLACEMENT_3D('',#4288,#3516,#3517);
#2935=AXIS2_PLACEMENT_3D('',#4289,#3518,#3519);
#2936=AXIS2_PLACEMENT_3D('',#4290,#3520,#3521);
#2937=AXIS2_PLACEMENT_3D('',#4292,#3522,#3523);
#2938=AXIS2_PLACEMENT_3D('',#4295,#3525,#3526);
#2939=AXIS2_PLACEMENT_3D('',#4296,#3527,#3528);
#2940=AXIS2_PLACEMENT_3D('',#4297,#3529,#3530);
#2941=AXIS2_PLACEMENT_3D('',#4299,#3531,#3532);
#2942=AXIS2_PLACEMENT_3D('',#4302,#3534,#3535);
#2943=AXIS2_PLACEMENT_3D('',#4303,#3536,#3537);
#2944=AXIS2_PLACEMENT_3D('',#4305,#3538,#3539);
#2945=AXIS2_PLACEMENT_3D('',#4308,#3541,#3542);
#2946=AXIS2_PLACEMENT_3D('',#4309,#3543,#3544);
#2947=AXIS2_PLACEMENT_3D('',#4318,#3549,#3550);
#2948=AXIS2_PLACEMENT_3D('',#4327,#3555,#3556);
#2949=AXIS2_PLACEMENT_3D('',#4338,#3563,#3564);
#2950=AXIS2_PLACEMENT_3D('',#4344,#3568,#3569);
#2951=AXIS2_PLACEMENT_3D('',#4348,#3572,#3573);
#2952=AXIS2_PLACEMENT_3D('',#4351,#3575,#3576);
#2953=AXIS2_PLACEMENT_3D('',#4352,#3577,#3578);
#2954=AXIS2_PLACEMENT_3D('',#4357,#3582,#3583);
#2955=AXIS2_PLACEMENT_3D('',#4358,#3584,#3585);
#2956=AXIS2_PLACEMENT_3D('',#4360,#3587,#3588);
#2957=AXIS2_PLACEMENT_3D('',#4361,#3589,#3590);
#2958=AXIS2_PLACEMENT_3D('',#4363,#3591,#3592);
#2959=AXIS2_PLACEMENT_3D('',#4365,#3594,#3595);
#2960=AXIS2_PLACEMENT_3D('',#4366,#3596,#3597);
#2961=AXIS2_PLACEMENT_3D('',#4367,#3598,#3599);
#2962=AXIS2_PLACEMENT_3D('',#4369,#3600,#3601);
#2963=AXIS2_PLACEMENT_3D('',#4372,#3603,#3604);
#2964=AXIS2_PLACEMENT_3D('',#4373,#3605,#3606);
#2965=AXIS2_PLACEMENT_3D('',#4375,#3607,#3608);
#2966=AXIS2_PLACEMENT_3D('',#4377,#3610,#3611);
#2967=AXIS2_PLACEMENT_3D('',#4378,#3612,#3613);
#2968=AXIS2_PLACEMENT_3D('',#4380,#3614,#3615);
#2969=AXIS2_PLACEMENT_3D('',#4406,#3617,#3618);
#2970=AXIS2_PLACEMENT_3D('',#4412,#3622,#3623);
#2971=AXIS2_PLACEMENT_3D('',#4416,#3626,#3627);
#2972=AXIS2_PLACEMENT_3D('',#4420,#3630,#3631);
#2973=AXIS2_PLACEMENT_3D('',#4424,#3634,#3635);
#2974=AXIS2_PLACEMENT_3D('',#4428,#3638,#3639);
#2975=AXIS2_PLACEMENT_3D('',#4430,#3641,#3642);
#2976=AXIS2_PLACEMENT_3D('',#4431,#3643,#3644);
#2977=AXIS2_PLACEMENT_3D('',#4432,#3645,#3646);
#2978=AXIS2_PLACEMENT_3D('',#4433,#3647,#3648);
#2979=AXIS2_PLACEMENT_3D('',#4445,#3650,#3651);
#2980=AXIS2_PLACEMENT_3D('',#4461,#3652,#3653);
#2981=AXIS2_PLACEMENT_3D('',#4463,#3654,#3655);
#2982=AXIS2_PLACEMENT_3D('',#4489,#3657,#3658);
#2983=AXIS2_PLACEMENT_3D('',#4492,#3661,#3662);
#2984=AXIS2_PLACEMENT_3D('',#4494,#3664,#3665);
#2985=AXIS2_PLACEMENT_3D('',#4496,#3667,#3668);
#2986=AXIS2_PLACEMENT_3D('',#4498,#3669,#3670);
#2987=AXIS2_PLACEMENT_3D('',#4501,#3672,#3673);
#2988=AXIS2_PLACEMENT_3D('',#4502,#3674,#3675);
#2989=AXIS2_PLACEMENT_3D('',#4504,#3677,#3678);
#2990=AXIS2_PLACEMENT_3D('',#4506,#3680,#3681);
#2991=AXIS2_PLACEMENT_3D('',#4507,#3682,#3683);
#2992=AXIS2_PLACEMENT_3D('',#4508,#3684,#3685);
#2993=AXIS2_PLACEMENT_3D('',#4509,#3686,#3687);
#2994=AXIS2_PLACEMENT_3D('',#4510,#3688,#3689);
#2995=AXIS2_PLACEMENT_3D('',#4512,#3690,#3691);
#2996=AXIS2_PLACEMENT_3D('',#4515,#3693,#3694);
#2997=AXIS2_PLACEMENT_3D('',#4516,#3695,#3696);
#2998=AXIS2_PLACEMENT_3D('',#4517,#3697,#3698);
#2999=AXIS2_PLACEMENT_3D('',#4518,#3699,#3700);
#3000=AXIS2_PLACEMENT_3D('',#4519,#3701,#3702);
#3001=AXIS2_PLACEMENT_3D('',#4597,#3704,#3705);
#3002=AXIS2_PLACEMENT_3D('',#4599,#3706,#3707);
#3003=AXIS2_PLACEMENT_3D('',#4600,#3708,#3709);
#3004=AXIS2_PLACEMENT_3D('',#4602,#3710,#3711);
#3005=AXIS2_PLACEMENT_3D('',#4604,#3713,#3714);
#3006=AXIS2_PLACEMENT_3D('',#4606,#3715,#3716);
#3007=AXIS2_PLACEMENT_3D('',#4608,#3718,#3719);
#3008=AXIS2_PLACEMENT_3D('',#4610,#3720,#3721);
#3009=AXIS2_PLACEMENT_3D('',#4611,#3722,#3723);
#3010=AXIS2_PLACEMENT_3D('',#4613,#3724,#3725);
#3011=AXIS2_PLACEMENT_3D('',#4616,#3728,#3729);
#3012=AXIS2_PLACEMENT_3D('',#4618,#3730,#3731);
#3013=AXIS2_PLACEMENT_3D('',#4620,#3733,#3734);
#3014=AXIS2_PLACEMENT_3D('',#4621,#3735,#3736);
#3015=AXIS2_PLACEMENT_3D('',#4622,#3737,#3738);
#3016=AXIS2_PLACEMENT_3D('',#4624,#3739,#3740);
#3017=AXIS2_PLACEMENT_3D('',#4627,#3742,#3743);
#3018=AXIS2_PLACEMENT_3D('',#4628,#3744,#3745);
#3019=AXIS2_PLACEMENT_3D('',#4630,#3746,#3747);
#3020=AXIS2_PLACEMENT_3D('',#4633,#3749,#3750);
#3021=AXIS2_PLACEMENT_3D('',#4634,#3751,#3752);
#3022=AXIS2_PLACEMENT_3D('',#4635,#3753,#3754);
#3023=AXIS2_PLACEMENT_3D('',#4636,#3755,#3756);
#3024=AXIS2_PLACEMENT_3D('',#4637,#3757,#3758);
#3025=AXIS2_PLACEMENT_3D('',#4639,#3759,#3760);
#3026=AXIS2_PLACEMENT_3D('',#4642,#3762,#3763);
#3027=AXIS2_PLACEMENT_3D('',#4643,#3764,#3765);
#3028=AXIS2_PLACEMENT_3D('',#4645,#3766,#3767);
#3029=AXIS2_PLACEMENT_3D('',#4648,#3769,#3770);
#3030=AXIS2_PLACEMENT_3D('',#4649,#3771,#3772);
#3031=AXIS2_PLACEMENT_3D('',#4650,#3773,#3774);
#3032=AXIS2_PLACEMENT_3D('',#4651,#3775,#3776);
#3033=AXIS2_PLACEMENT_3D('',#4652,#3777,#3778);
#3034=AXIS2_PLACEMENT_3D('',#4654,#3779,#3780);
#3035=AXIS2_PLACEMENT_3D('',#4655,#3781,#3782);
#3036=AXIS2_PLACEMENT_3D('',#4710,#3783,#3784);
#3037=AXIS2_PLACEMENT_3D('',#4713,#3785,#3786);
#3038=AXIS2_PLACEMENT_3D('',#4715,#3788,#3789);
#3039=AXIS2_PLACEMENT_3D('',#4721,#3793,#3794);
#3040=AXIS2_PLACEMENT_3D('',#4723,#3795,#3796);
#3041=AXIS2_PLACEMENT_3D('',#4725,#3798,#3799);
#3042=AXIS2_PLACEMENT_3D('',#4726,#3800,#3801);
#3043=AXIS2_PLACEMENT_3D('',#4727,#3802,#3803);
#3044=AXIS2_PLACEMENT_3D('',#4728,#3804,#3805);
#3045=AXIS2_PLACEMENT_3D('',#4729,#3806,#3807);
#3046=AXIS2_PLACEMENT_3D('',#4730,#3808,#3809);
#3047=AXIS2_PLACEMENT_3D('',#4731,#3810,#3811);
#3048=AXIS2_PLACEMENT_3D('',#4732,#3812,#3813);
#3049=AXIS2_PLACEMENT_3D('',#4733,#3814,#3815);
#3050=AXIS2_PLACEMENT_3D('',#4734,#3816,#3817);
#3051=AXIS2_PLACEMENT_3D('',#4735,#3818,#3819);
#3052=AXIS2_PLACEMENT_3D('',#4736,#3820,#3821);
#3053=AXIS2_PLACEMENT_3D('',#4737,#3822,#3823);
#3054=AXIS2_PLACEMENT_3D('',#4738,#3824,#3825);
#3055=AXIS2_PLACEMENT_3D('',#4739,#3826,#3827);
#3056=AXIS2_PLACEMENT_3D('',#4740,#3828,#3829);
#3057=AXIS2_PLACEMENT_3D('',#4741,#3830,#3831);
#3058=AXIS2_PLACEMENT_3D('',#4742,#3832,#3833);
#3059=AXIS2_PLACEMENT_3D('',#4743,#3834,#3835);
#3060=AXIS2_PLACEMENT_3D('',#4744,#3836,#3837);
#3061=AXIS2_PLACEMENT_3D('',#4745,#3838,#3839);
#3062=AXIS2_PLACEMENT_3D('',#4746,#3840,#3841);
#3063=AXIS2_PLACEMENT_3D('',#4747,#3842,#3843);
#3064=AXIS2_PLACEMENT_3D('',#4748,#3844,#3845);
#3065=AXIS2_PLACEMENT_3D('',#4749,#3846,#3847);
#3066=AXIS2_PLACEMENT_3D('',#4750,#3848,#3849);
#3067=AXIS2_PLACEMENT_3D('',#4751,#3850,#3851);
#3068=AXIS2_PLACEMENT_3D('',#4752,#3852,#3853);
#3069=AXIS2_PLACEMENT_3D('',#4753,#3854,#3855);
#3070=DIRECTION('axis',(0.,0.,1.));
#3071=DIRECTION('refdir',(1.,0.,0.));
#3072=DIRECTION('axis',(0.,0.,1.));
#3073=DIRECTION('refdir',(1.,0.,0.));
#3074=DIRECTION('axis',(0.,0.,1.));
#3075=DIRECTION('refdir',(1.,0.,0.));
#3076=DIRECTION('center_axis',(0.,1.,0.));
#3077=DIRECTION('ref_axis',(1.,0.,0.));
#3078=DIRECTION('',(0.,1.,0.));
#3079=DIRECTION('center_axis',(0.,1.,0.));
#3080=DIRECTION('ref_axis',(1.,0.,0.));
#3081=DIRECTION('',(0.,1.,0.));
#3082=DIRECTION('center_axis',(0.,1.,0.));
#3083=DIRECTION('ref_axis',(1.,0.,0.));
#3084=DIRECTION('',(0.,-1.,0.));
#3085=DIRECTION('center_axis',(0.,1.,0.));
#3086=DIRECTION('ref_axis',(1.,0.,0.));
#3087=DIRECTION('center_axis',(0.,1.,0.));
#3088=DIRECTION('ref_axis',(1.,0.,0.));
#3089=DIRECTION('center_axis',(0.,1.,0.));
#3090=DIRECTION('ref_axis',(1.,0.,0.));
#3091=DIRECTION('center_axis',(0.,1.,0.));
#3092=DIRECTION('ref_axis',(-1.,0.,0.));
#3093=DIRECTION('',(1.,0.,0.));
#3094=DIRECTION('',(0.,0.,-1.));
#3095=DIRECTION('',(-1.,0.,0.));
#3096=DIRECTION('',(0.,0.,1.));
#3097=DIRECTION('',(-1.,0.,0.));
#3098=DIRECTION('',(0.,0.,1.));
#3099=DIRECTION('',(-1.,0.,0.));
#3100=DIRECTION('',(0.,0.,1.));
#3101=DIRECTION('',(-1.,0.,0.));
#3102=DIRECTION('center_axis',(0.,0.,-1.));
#3103=DIRECTION('ref_axis',(-1.,0.,0.));
#3104=DIRECTION('',(0.,1.,0.));
#3105=DIRECTION('',(1.,0.,0.));
#3106=DIRECTION('center_axis',(0.,0.,1.));
#3107=DIRECTION('ref_axis',(1.,0.,0.));
#3108=DIRECTION('',(-1.,0.,0.));
#3109=DIRECTION('',(0.,1.,0.));
#3110=DIRECTION('center_axis',(1.,0.,0.));
#3111=DIRECTION('ref_axis',(0.,0.,-1.));
#3112=DIRECTION('',(0.,0.,1.));
#3113=DIRECTION('',(0.,-1.,0.));
#3114=DIRECTION('center_axis',(-1.,0.,0.));
#3115=DIRECTION('ref_axis',(0.,0.,1.));
#3116=DIRECTION('',(0.,1.,0.));
#3117=DIRECTION('',(0.,0.,-1.));
#3118=DIRECTION('center_axis',(0.,1.,0.));
#3119=DIRECTION('ref_axis',(1.,0.,0.));
#3120=DIRECTION('',(-1.,0.,0.));
#3121=DIRECTION('center_axis',(0.,0.,1.));
#3122=DIRECTION('ref_axis',(1.,0.,0.));
#3123=DIRECTION('',(0.,-1.,0.));
#3124=DIRECTION('',(1.,0.,0.));
#3125=DIRECTION('',(0.,1.,0.));
#3126=DIRECTION('',(0.,-1.,0.));
#3127=DIRECTION('',(-1.,0.,0.));
#3128=DIRECTION('',(0.,1.,0.));
#3129=DIRECTION('',(1.,0.,0.));
#3130=DIRECTION('',(0.,-1.,0.));
#3131=DIRECTION('',(-1.,0.,0.));
#3132=DIRECTION('',(0.,1.,0.));
#3133=DIRECTION('',(1.,0.,0.));
#3134=DIRECTION('',(0.,-1.,0.));
#3135=DIRECTION('',(-1.,0.,0.));
#3136=DIRECTION('',(0.,1.,0.));
#3137=DIRECTION('',(1.,0.,0.));
#3138=DIRECTION('center_axis',(0.,0.,-1.));
#3139=DIRECTION('ref_axis',(1.,0.,0.));
#3140=DIRECTION('center_axis',(0.,0.,-1.));
#3141=DIRECTION('ref_axis',(1.,0.,0.));
#3142=DIRECTION('center_axis',(0.,0.,1.));
#3143=DIRECTION('ref_axis',(1.,0.,0.));
#3144=DIRECTION('center_axis',(0.,0.,1.));
#3145=DIRECTION('ref_axis',(1.,0.,0.));
#3146=DIRECTION('',(0.,0.,1.));
#3147=DIRECTION('center_axis',(0.,0.,1.));
#3148=DIRECTION('ref_axis',(1.,0.,0.));
#3149=DIRECTION('center_axis',(0.,0.,1.));
#3150=DIRECTION('ref_axis',(1.,0.,0.));
#3151=DIRECTION('',(0.,0.,1.));
#3152=DIRECTION('center_axis',(1.,0.,0.));
#3153=DIRECTION('ref_axis',(0.,0.,-1.));
#3154=DIRECTION('center_axis',(1.,0.,0.));
#3155=DIRECTION('ref_axis',(0.,0.,-1.));
#3156=DIRECTION('',(1.,0.,0.));
#3157=DIRECTION('center_axis',(-1.,0.,0.));
#3158=DIRECTION('ref_axis',(0.,0.,-1.));
#3159=DIRECTION('center_axis',(0.,1.,0.));
#3160=DIRECTION('ref_axis',(1.,0.,0.));
#3161=DIRECTION('',(0.,0.,1.));
#3162=DIRECTION('',(-1.,0.,0.));
#3163=DIRECTION('',(0.,0.,-1.));
#3164=DIRECTION('center_axis',(1.,0.,0.));
#3165=DIRECTION('ref_axis',(0.,0.,-1.));
#3166=DIRECTION('',(0.,0.,-1.));
#3167=DIRECTION('',(0.,1.,0.));
#3168=DIRECTION('center_axis',(-1.,0.,0.));
#3169=DIRECTION('ref_axis',(0.,0.,1.));
#3170=DIRECTION('',(0.,1.,0.));
#3171=DIRECTION('',(0.,0.,1.));
#3172=DIRECTION('center_axis',(0.,0.,1.));
#3173=DIRECTION('ref_axis',(1.,0.,0.));
#3174=DIRECTION('',(1.,0.,0.));
#3175=DIRECTION('center_axis',(0.,1.,0.));
#3176=DIRECTION('ref_axis',(0.,0.,1.));
#3177=DIRECTION('center_axis',(0.,1.,0.));
#3178=DIRECTION('ref_axis',(1.,0.,0.));
#3179=DIRECTION('center_axis',(0.,1.,0.));
#3180=DIRECTION('ref_axis',(1.,0.,0.));
#3181=DIRECTION('',(0.,1.,0.));
#3182=DIRECTION('center_axis',(0.,-1.,0.));
#3183=DIRECTION('ref_axis',(1.,0.,0.));
#3184=DIRECTION('center_axis',(0.,1.,0.));
#3185=DIRECTION('ref_axis',(1.,0.,0.));
#3186=DIRECTION('center_axis',(0.,1.,0.));
#3187=DIRECTION('ref_axis',(1.,0.,0.));
#3188=DIRECTION('',(0.,1.,0.));
#3189=DIRECTION('center_axis',(0.,-1.,0.));
#3190=DIRECTION('ref_axis',(1.,0.,0.));
#3191=DIRECTION('center_axis',(0.,1.,0.));
#3192=DIRECTION('ref_axis',(1.,0.,0.));
#3193=DIRECTION('',(0.,0.,1.));
#3194=DIRECTION('',(-1.,0.,0.));
#3195=DIRECTION('',(0.,0.,-1.));
#3196=DIRECTION('center_axis',(1.,0.,0.));
#3197=DIRECTION('ref_axis',(0.,0.,-1.));
#3198=DIRECTION('',(0.,0.,-1.));
#3199=DIRECTION('',(0.,1.,0.));
#3200=DIRECTION('center_axis',(-1.,0.,0.));
#3201=DIRECTION('ref_axis',(0.,0.,1.));
#3202=DIRECTION('',(0.,1.,0.));
#3203=DIRECTION('',(0.,0.,1.));
#3204=DIRECTION('center_axis',(0.,0.,1.));
#3205=DIRECTION('ref_axis',(1.,0.,0.));
#3206=DIRECTION('',(1.,0.,0.));
#3207=DIRECTION('center_axis',(0.,1.,0.));
#3208=DIRECTION('ref_axis',(0.,0.,1.));
#3209=DIRECTION('center_axis',(0.,1.,0.));
#3210=DIRECTION('ref_axis',(1.,0.,0.));
#3211=DIRECTION('',(0.,0.,1.));
#3212=DIRECTION('',(-1.,0.,0.));
#3213=DIRECTION('',(0.,0.,-1.));
#3214=DIRECTION('center_axis',(1.,0.,0.));
#3215=DIRECTION('ref_axis',(0.,0.,-1.));
#3216=DIRECTION('',(0.,0.,-1.));
#3217=DIRECTION('',(0.,1.,0.));
#3218=DIRECTION('center_axis',(-1.,0.,0.));
#3219=DIRECTION('ref_axis',(0.,0.,1.));
#3220=DIRECTION('',(0.,1.,0.));
#3221=DIRECTION('',(0.,0.,1.));
#3222=DIRECTION('center_axis',(0.,0.,1.));
#3223=DIRECTION('ref_axis',(1.,0.,0.));
#3224=DIRECTION('',(1.,0.,0.));
#3225=DIRECTION('center_axis',(0.,1.,0.));
#3226=DIRECTION('ref_axis',(0.,0.,1.));
#3227=DIRECTION('center_axis',(1.,0.,0.));
#3228=DIRECTION('ref_axis',(0.,1.,0.));
#3229=DIRECTION('',(0.,1.,0.));
#3230=DIRECTION('',(0.,0.,1.));
#3231=DIRECTION('center_axis',(0.,-1.,0.));
#3232=DIRECTION('ref_axis',(1.,0.,0.));
#3233=DIRECTION('',(1.,0.,0.));
#3234=DIRECTION('',(0.,0.,1.));
#3235=DIRECTION('center_axis',(-1.,0.,0.));
#3236=DIRECTION('ref_axis',(0.,-1.,0.));
#3237=DIRECTION('',(0.,-1.,0.));
#3238=DIRECTION('center_axis',(0.,0.,1.));
#3239=DIRECTION('ref_axis',(1.,0.,0.));
#3240=DIRECTION('axis',(0.,0.,1.));
#3241=DIRECTION('refdir',(1.,0.,0.));
#3242=DIRECTION('axis',(0.,0.,1.));
#3243=DIRECTION('refdir',(1.,0.,0.));
#3244=DIRECTION('center_axis',(0.,1.,0.));
#3245=DIRECTION('ref_axis',(1.,0.,0.));
#3246=DIRECTION('center_axis',(0.,1.,0.));
#3247=DIRECTION('ref_axis',(1.,0.,0.));
#3248=DIRECTION('',(0.,1.,0.));
#3249=DIRECTION('center_axis',(0.,-1.,0.));
#3250=DIRECTION('ref_axis',(1.,0.,0.));
#3251=DIRECTION('center_axis',(0.,1.,0.));
#3252=DIRECTION('ref_axis',(1.,0.,0.));
#3253=DIRECTION('center_axis',(0.,1.,0.));
#3254=DIRECTION('ref_axis',(1.,0.,0.));
#3255=DIRECTION('',(0.,1.,0.));
#3256=DIRECTION('center_axis',(0.,-1.,0.));
#3257=DIRECTION('ref_axis',(1.,0.,0.));
#3258=DIRECTION('center_axis',(0.,1.,0.));
#3259=DIRECTION('ref_axis',(0.0871557427476581,0.,0.996194698091746));
#3260=DIRECTION('',(0.,-1.,0.));
#3261=DIRECTION('center_axis',(0.,1.,0.));
#3262=DIRECTION('ref_axis',(1.,0.,0.));
#3263=DIRECTION('',(0.,1.,0.));
#3264=DIRECTION('center_axis',(0.,1.,0.));
#3265=DIRECTION('ref_axis',(1.,0.,0.));
#3266=DIRECTION('center_axis',(0.,1.,0.));
#3267=DIRECTION('ref_axis',(1.,0.,0.));
#3268=DIRECTION('',(0.0871557427476582,0.,0.996194698091746));
#3269=DIRECTION('center_axis',(0.,-1.,0.));
#3270=DIRECTION('ref_axis',(1.,0.,0.));
#3271=DIRECTION('',(-0.0871557427476581,0.,-0.996194698091746));
#3272=DIRECTION('center_axis',(-0.996194698091746,0.,0.0871557427476582));
#3273=DIRECTION('ref_axis',(0.0871557427476582,0.,0.996194698091746));
#3274=DIRECTION('',(0.0871557427476582,0.,0.996194698091746));
#3275=DIRECTION('',(0.,1.,0.));
#3276=DIRECTION('center_axis',(0.,1.,0.));
#3277=DIRECTION('ref_axis',(0.,0.,1.));
#3278=DIRECTION('',(-0.0871557427476581,0.,-0.996194698091746));
#3279=DIRECTION('center_axis',(0.,1.,0.));
#3280=DIRECTION('ref_axis',(1.,0.,0.));
#3281=DIRECTION('center_axis',(0.996194698091746,0.,-0.0871557427476581));
#3282=DIRECTION('ref_axis',(-0.0871557427476581,0.,-0.996194698091746));
#3283=DIRECTION('',(0.,-1.,0.));
#3284=DIRECTION('center_axis',(0.,1.,0.));
#3285=DIRECTION('ref_axis',(1.,0.,0.));
#3286=DIRECTION('center_axis',(0.,1.,0.));
#3287=DIRECTION('ref_axis',(1.,0.,0.));
#3288=DIRECTION('',(0.,1.,0.));
#3289=DIRECTION('center_axis',(0.,-1.,0.));
#3290=DIRECTION('ref_axis',(1.,0.,0.));
#3291=DIRECTION('center_axis',(0.,1.,0.));
#3292=DIRECTION('ref_axis',(1.,0.,0.));
#3293=DIRECTION('center_axis',(0.,1.,0.));
#3294=DIRECTION('ref_axis',(1.,0.,0.));
#3295=DIRECTION('',(0.,1.,0.));
#3296=DIRECTION('center_axis',(0.,-1.,0.));
#3297=DIRECTION('ref_axis',(1.,0.,0.));
#3298=DIRECTION('center_axis',(0.996194698091746,0.,-0.0871557427476583));
#3299=DIRECTION('ref_axis',(-0.0871557427476583,0.,-0.996194698091746));
#3300=DIRECTION('',(0.0871557427476583,0.,0.996194698091746));
#3301=DIRECTION('',(0.,1.,0.));
#3302=DIRECTION('',(-0.0871557427476583,0.,-0.996194698091746));
#3303=DIRECTION('',(0.,1.,0.));
#3304=DIRECTION('center_axis',(0.,1.,0.));
#3305=DIRECTION('ref_axis',(0.,0.,1.));
#3306=DIRECTION('',(0.996194698091746,0.,-0.0871557427476581));
#3307=DIRECTION('',(-0.087155742747658,0.,-0.996194698091746));
#3308=DIRECTION('',(-0.996194698091746,0.,0.0871557427476581));
#3309=DIRECTION('',(0.0871557427476582,0.,0.996194698091746));
#3310=DIRECTION('center_axis',(0.996194698091746,0.,-0.087155742747658));
#3311=DIRECTION('ref_axis',(-0.087155742747658,0.,-0.996194698091746));
#3312=DIRECTION('',(0.087155742747658,0.,0.996194698091746));
#3313=DIRECTION('',(0.,1.,0.));
#3314=DIRECTION('',(0.,1.,0.));
#3315=DIRECTION('center_axis',(0.,1.,0.));
#3316=DIRECTION('ref_axis',(1.,0.,0.));
#3317=DIRECTION('',(0.996194698091746,0.,-0.0871557427476581));
#3318=DIRECTION('',(-0.996194698091746,0.,0.0871557427476581));
#3319=DIRECTION('center_axis',(0.,1.,0.));
#3320=DIRECTION('ref_axis',(1.,0.,0.));
#3321=DIRECTION('',(0.0871557427476582,0.,0.996194698091746));
#3322=DIRECTION('',(0.996194698091746,0.,-0.0871557427476581));
#3323=DIRECTION('center_axis',(0.,-1.,0.));
#3324=DIRECTION('ref_axis',(1.,0.,0.));
#3325=DIRECTION('',(-0.996194698091746,0.,0.087155742747658));
#3326=DIRECTION('center_axis',(0.0871557427476581,0.,0.996194698091746));
#3327=DIRECTION('ref_axis',(0.996194698091746,0.,-0.0871557427476581));
#3328=DIRECTION('',(0.,1.,0.));
#3329=DIRECTION('',(0.996194698091746,0.,-0.0871557427476581));
#3330=DIRECTION('',(0.,1.,0.));
#3331=DIRECTION('center_axis',(0.,1.,0.));
#3332=DIRECTION('ref_axis',(0.,0.,1.));
#3333=DIRECTION('',(-0.0871557427476582,0.,-0.996194698091746));
#3334=DIRECTION('',(-0.996194698091746,0.,0.087155742747658));
#3335=DIRECTION('center_axis',(0.,1.,0.));
#3336=DIRECTION('ref_axis',(1.,0.,0.));
#3337=DIRECTION('center_axis',(-0.087155742747658,0.,-0.996194698091746));
#3338=DIRECTION('ref_axis',(-0.996194698091746,0.,0.087155742747658));
#3339=DIRECTION('',(0.,-1.,0.));
#3340=DIRECTION('',(0.,-1.,0.));
#3341=DIRECTION('center_axis',(0.,1.,0.));
#3342=DIRECTION('ref_axis',(1.,0.,0.));
#3343=DIRECTION('center_axis',(0.,1.,0.));
#3344=DIRECTION('ref_axis',(1.,0.,0.));
#3345=DIRECTION('',(0.,-1.,0.));
#3346=DIRECTION('center_axis',(0.,1.,0.));
#3347=DIRECTION('ref_axis',(1.,0.,0.));
#3348=DIRECTION('center_axis',(0.,1.,0.));
#3349=DIRECTION('ref_axis',(1.,0.,0.));
#3350=DIRECTION('center_axis',(0.,1.,0.));
#3351=DIRECTION('ref_axis',(1.,0.,0.));
#3352=DIRECTION('center_axis',(-0.0871557427476581,0.,-0.996194698091746));
#3353=DIRECTION('ref_axis',(-0.996194698091746,0.,0.0871557427476581));
#3354=DIRECTION('',(-0.996194698091746,0.,0.0871557427476581));
#3355=DIRECTION('',(0.,1.,0.));
#3356=DIRECTION('',(0.996194698091746,0.,-0.0871557427476581));
#3357=DIRECTION('',(0.,1.,0.));
#3358=DIRECTION('center_axis',(0.,1.,0.));
#3359=DIRECTION('ref_axis',(0.,0.,1.));
#3360=DIRECTION('',(0.996194698091746,0.,-0.0871557427476581));
#3361=DIRECTION('',(-0.087155742747658,0.,-0.996194698091746));
#3362=DIRECTION('center_axis',(-0.996194698091746,0.,0.0871557427476582));
#3363=DIRECTION('ref_axis',(0.0871557427476582,0.,0.996194698091746));
#3364=DIRECTION('',(-0.0871557427476582,0.,-0.996194698091746));
#3365=DIRECTION('',(0.,1.,0.));
#3366=DIRECTION('center_axis',(0.996194698091746,0.,-0.087155742747658));
#3367=DIRECTION('ref_axis',(-0.087155742747658,0.,-0.996194698091746));
#3368=DIRECTION('',(0.087155742747658,0.,0.996194698091746));
#3369=DIRECTION('',(0.,1.,0.));
#3370=DIRECTION('center_axis',(0.0871557427476581,0.,0.996194698091746));
#3371=DIRECTION('ref_axis',(0.996194698091746,0.,-0.0871557427476581));
#3372=DIRECTION('',(-0.996194698091746,0.,0.0871557427476581));
#3373=DIRECTION('center_axis',(0.,1.,0.));
#3374=DIRECTION('ref_axis',(1.,0.,0.));
#3375=DIRECTION('axis',(0.,0.,1.));
#3376=DIRECTION('refdir',(1.,0.,0.));
#3377=DIRECTION('center_axis',(0.,1.,0.));
#3378=DIRECTION('ref_axis',(1.,0.,0.));
#3379=DIRECTION('center_axis',(0.,1.,0.));
#3380=DIRECTION('ref_axis',(1.,0.,0.));
#3381=DIRECTION('',(0.,1.,0.));
#3382=DIRECTION('center_axis',(0.,-1.,0.));
#3383=DIRECTION('ref_axis',(1.,0.,0.));
#3384=DIRECTION('center_axis',(0.,1.,0.));
#3385=DIRECTION('ref_axis',(1.,0.,0.));
#3386=DIRECTION('center_axis',(0.,1.,0.));
#3387=DIRECTION('ref_axis',(1.,0.,0.));
#3388=DIRECTION('center_axis',(0.,1.,0.));
#3389=DIRECTION('ref_axis',(1.,0.,0.));
#3390=DIRECTION('',(0.,-1.,0.));
#3391=DIRECTION('center_axis',(0.,1.,0.));
#3392=DIRECTION('ref_axis',(1.,0.,0.));
#3393=DIRECTION('center_axis',(0.,1.,0.));
#3394=DIRECTION('ref_axis',(1.,0.,0.));
#3395=DIRECTION('center_axis',(0.,1.,0.));
#3396=DIRECTION('ref_axis',(1.,0.,0.));
#3397=DIRECTION('axis',(0.,0.,1.));
#3398=DIRECTION('refdir',(1.,0.,0.));
#3399=DIRECTION('center_axis',(0.866025403784439,0.,-0.5));
#3400=DIRECTION('ref_axis',(0.5,0.,0.866025403784439));
#3401=DIRECTION('',(-0.5,0.,-0.866025403784439));
#3402=DIRECTION('',(0.,-1.,0.));
#3403=DIRECTION('',(0.5,0.,0.866025403784439));
#3404=DIRECTION('',(0.,-1.,0.));
#3405=DIRECTION('center_axis',(1.20185167898973E-16,0.,-1.));
#3406=DIRECTION('ref_axis',(1.,0.,1.20185167898973E-16));
#3407=DIRECTION('',(-1.,0.,-1.20185167898973E-16));
#3408=DIRECTION('',(0.,-1.,0.));
#3409=DIRECTION('',(1.,0.,1.20185167898973E-16));
#3410=DIRECTION('center_axis',(-0.866025403784439,0.,-0.5));
#3411=DIRECTION('ref_axis',(0.5,0.,-0.866025403784439));
#3412=DIRECTION('',(-0.5,0.,0.866025403784439));
#3413=DIRECTION('',(0.,-1.,0.));
#3414=DIRECTION('',(0.5,0.,-0.866025403784439));
#3415=DIRECTION('center_axis',(-0.866025403784439,0.,0.5));
#3416=DIRECTION('ref_axis',(-0.5,0.,-0.866025403784439));
#3417=DIRECTION('',(0.5,0.,0.866025403784439));
#3418=DIRECTION('',(0.,-1.,0.));
#3419=DIRECTION('',(-0.5,0.,-0.866025403784439));
#3420=DIRECTION('center_axis',(-2.40370335797945E-16,0.,1.));
#3421=DIRECTION('ref_axis',(-1.,0.,-2.40370335797945E-16));
#3422=DIRECTION('',(1.,0.,2.40370335797945E-16));
#3423=DIRECTION('',(0.,-1.,0.));
#3424=DIRECTION('',(-1.,0.,-2.40370335797945E-16));
#3425=DIRECTION('center_axis',(0.866025403784439,0.,0.5));
#3426=DIRECTION('ref_axis',(-0.5,0.,0.866025403784439));
#3427=DIRECTION('',(0.5,0.,-0.866025403784439));
#3428=DIRECTION('',(-0.5,0.,0.866025403784439));
#3429=DIRECTION('center_axis',(0.,1.,0.));
#3430=DIRECTION('ref_axis',(1.,0.,0.));
#3431=DIRECTION('center_axis',(0.,-1.,0.));
#3432=DIRECTION('ref_axis',(0.,0.,-1.));
#3433=DIRECTION('center_axis',(0.,1.,0.));
#3434=DIRECTION('ref_axis',(1.,0.,0.));
#3435=DIRECTION('center_axis',(0.,1.,0.));
#3436=DIRECTION('ref_axis',(1.,0.,0.));
#3437=DIRECTION('center_axis',(0.,1.,0.));
#3438=DIRECTION('ref_axis',(0.,0.,1.));
#3439=DIRECTION('center_axis',(0.,-1.,0.));
#3440=DIRECTION('ref_axis',(1.,0.,0.));
#3441=DIRECTION('center_axis',(0.,-1.,0.));
#3442=DIRECTION('ref_axis',(1.,0.,0.));
#3443=DIRECTION('center_axis',(0.,-1.,0.));
#3444=DIRECTION('ref_axis',(1.,0.,0.));
#3445=DIRECTION('',(0.707106781186548,0.707106781186547,8.65956056235493E-17));
#3446=DIRECTION('center_axis',(0.,-1.,0.));
#3447=DIRECTION('ref_axis',(1.,0.,0.));
#3448=DIRECTION('center_axis',(0.,-1.,0.));
#3449=DIRECTION('ref_axis',(1.,0.,0.));
#3450=DIRECTION('',(0.,1.,0.));
#3451=DIRECTION('center_axis',(0.,1.,0.));
#3452=DIRECTION('ref_axis',(1.,0.,0.));
#3453=DIRECTION('center_axis',(0.,-1.,0.));
#3454=DIRECTION('ref_axis',(1.,0.,0.));
#3455=DIRECTION('',(-0.707106781186547,0.707106781186548,-8.65956056235493E-17));
#3456=DIRECTION('center_axis',(0.,-1.,0.));
#3457=DIRECTION('ref_axis',(0.,0.,-1.));
#3458=DIRECTION('center_axis',(0.,-1.,0.));
#3459=DIRECTION('ref_axis',(1.,0.,0.));
#3460=DIRECTION('center_axis',(0.,1.,0.));
#3461=DIRECTION('ref_axis',(1.,0.,0.));
#3462=DIRECTION('center_axis',(0.,1.,0.));
#3463=DIRECTION('ref_axis',(1.,0.,0.));
#3464=DIRECTION('',(-0.447213595499958,0.894427190999916,-5.47678698264203E-17));
#3465=DIRECTION('center_axis',(0.,-1.,0.));
#3466=DIRECTION('ref_axis',(1.,0.,0.));
#3467=DIRECTION('',(0.,1.,0.));
#3468=DIRECTION('axis',(0.,0.,1.));
#3469=DIRECTION('refdir',(1.,0.,0.));
#3470=DIRECTION('axis',(0.,0.,1.));
#3471=DIRECTION('refdir',(1.,0.,0.));
#3472=DIRECTION('center_axis',(0.,1.,0.));
#3473=DIRECTION('ref_axis',(1.,0.,0.));
#3474=DIRECTION('center_axis',(0.,1.,0.));
#3475=DIRECTION('ref_axis',(1.,0.,0.));
#3476=DIRECTION('',(0.,1.,0.));
#3477=DIRECTION('center_axis',(0.,-1.,0.));
#3478=DIRECTION('ref_axis',(1.,0.,0.));
#3479=DIRECTION('center_axis',(0.,1.,0.));
#3480=DIRECTION('ref_axis',(1.,0.,0.));
#3481=DIRECTION('center_axis',(0.,1.,0.));
#3482=DIRECTION('ref_axis',(1.,0.,0.));
#3483=DIRECTION('',(0.,1.,0.));
#3484=DIRECTION('center_axis',(0.,-1.,0.));
#3485=DIRECTION('ref_axis',(1.,0.,0.));
#3486=DIRECTION('center_axis',(0.,1.,0.));
#3487=DIRECTION('ref_axis',(1.,0.,0.));
#3488=DIRECTION('',(0.,-1.,0.));
#3489=DIRECTION('center_axis',(0.,1.,0.));
#3490=DIRECTION('ref_axis',(1.,0.,0.));
#3491=DIRECTION('',(0.,1.,0.));
#3492=DIRECTION('center_axis',(0.,1.,0.));
#3493=DIRECTION('ref_axis',(1.,0.,0.));
#3494=DIRECTION('center_axis',(0.062254101962613,0.,-0.998060332238903));
#3495=DIRECTION('ref_axis',(-0.998060332238903,0.,-0.062254101962613));
#3496=DIRECTION('',(-0.998060332238903,0.,-0.062254101962613));
#3497=DIRECTION('',(0.,-1.,0.));
#3498=DIRECTION('',(-0.998060332238903,0.,-0.062254101962613));
#3499=DIRECTION('center_axis',(0.,1.,0.));
#3500=DIRECTION('ref_axis',(1.,0.,0.));
#3501=DIRECTION('',(0.998060332238903,0.,0.062254101962613));
#3502=DIRECTION('center_axis',(0.,1.,0.));
#3503=DIRECTION('ref_axis',(1.,0.,0.));
#3504=DIRECTION('center_axis',(-0.062254101962613,0.,0.998060332238903));
#3505=DIRECTION('ref_axis',(0.998060332238903,0.,0.062254101962613));
#3506=DIRECTION('',(0.998060332238903,0.,0.062254101962613));
#3507=DIRECTION('',(0.,1.,0.));
#3508=DIRECTION('center_axis',(0.,1.,0.));
#3509=DIRECTION('ref_axis',(-0.998060332238903,0.,-0.0622541019626133));
#3510=DIRECTION('center_axis',(0.,1.,0.));
#3511=DIRECTION('ref_axis',(1.,0.,0.));
#3512=DIRECTION('center_axis',(0.,1.,0.));
#3513=DIRECTION('ref_axis',(1.,0.,0.));
#3514=DIRECTION('',(0.,0.,1.));
#3515=DIRECTION('',(1.,0.,0.));
#3516=DIRECTION('axis',(0.,0.,1.));
#3517=DIRECTION('refdir',(1.,0.,0.));
#3518=DIRECTION('axis',(0.,0.,1.));
#3519=DIRECTION('refdir',(1.,0.,0.));
#3520=DIRECTION('center_axis',(1.,0.,0.));
#3521=DIRECTION('ref_axis',(0.,0.,-1.));
#3522=DIRECTION('center_axis',(1.,0.,0.));
#3523=DIRECTION('ref_axis',(0.,0.,-1.));
#3524=DIRECTION('',(1.,0.,0.));
#3525=DIRECTION('center_axis',(-1.,0.,0.));
#3526=DIRECTION('ref_axis',(0.,0.,-1.));
#3527=DIRECTION('center_axis',(1.,0.,0.));
#3528=DIRECTION('ref_axis',(0.,0.,-1.));
#3529=DIRECTION('center_axis',(0.,1.,0.));
#3530=DIRECTION('ref_axis',(1.,0.,0.));
#3531=DIRECTION('center_axis',(0.,1.,0.));
#3532=DIRECTION('ref_axis',(1.,0.,0.));
#3533=DIRECTION('',(0.,1.,0.));
#3534=DIRECTION('center_axis',(0.,-1.,0.));
#3535=DIRECTION('ref_axis',(1.,0.,0.));
#3536=DIRECTION('center_axis',(0.,1.,0.));
#3537=DIRECTION('ref_axis',(1.,0.,0.));
#3538=DIRECTION('center_axis',(0.,1.,0.));
#3539=DIRECTION('ref_axis',(1.,0.,0.));
#3540=DIRECTION('',(0.,1.,0.));
#3541=DIRECTION('center_axis',(0.,-1.,0.));
#3542=DIRECTION('ref_axis',(1.,0.,0.));
#3543=DIRECTION('center_axis',(-1.,0.,0.));
#3544=DIRECTION('ref_axis',(0.,0.,1.));
#3545=DIRECTION('',(0.,0.,1.));
#3546=DIRECTION('',(0.,1.,0.));
#3547=DIRECTION('',(0.,0.,-1.));
#3548=DIRECTION('',(0.,1.,0.));
#3549=DIRECTION('center_axis',(0.,1.,0.));
#3550=DIRECTION('ref_axis',(0.,0.,1.));
#3551=DIRECTION('',(-1.,0.,0.));
#3552=DIRECTION('',(0.,0.,1.));
#3553=DIRECTION('',(1.,0.,0.));
#3554=DIRECTION('',(0.,0.,-1.));
#3555=DIRECTION('center_axis',(0.,0.,-1.));
#3556=DIRECTION('ref_axis',(-1.,0.,0.));
#3557=DIRECTION('',(1.,0.,0.));
#3558=DIRECTION('',(0.,1.,0.));
#3559=DIRECTION('',(0.,1.,0.));
#3560=DIRECTION('',(1.,0.,0.));
#3561=DIRECTION('',(0.,1.,0.));
#3562=DIRECTION('',(-1.,0.,0.));
#3563=DIRECTION('center_axis',(0.,1.,0.));
#3564=DIRECTION('ref_axis',(1.,0.,0.));
#3565=DIRECTION('',(-1.,0.,0.));
#3566=DIRECTION('',(0.,0.,-1.));
#3567=DIRECTION('',(0.,0.,1.));
#3568=DIRECTION('center_axis',(-1.,0.,0.));
#3569=DIRECTION('ref_axis',(0.,0.,1.));
#3570=DIRECTION('',(0.,0.,-1.));
#3571=DIRECTION('',(0.,1.,0.));
#3572=DIRECTION('center_axis',(1.,0.,0.));
#3573=DIRECTION('ref_axis',(0.,0.,-1.));
#3574=DIRECTION('',(0.,1.,0.));
#3575=DIRECTION('center_axis',(1.,0.,0.));
#3576=DIRECTION('ref_axis',(0.,0.,-1.));
#3577=DIRECTION('center_axis',(0.,0.,1.));
#3578=DIRECTION('ref_axis',(1.,0.,0.));
#3579=DIRECTION('',(-1.,0.,0.));
#3580=DIRECTION('',(1.,0.,0.));
#3581=DIRECTION('',(0.,1.,0.));
#3582=DIRECTION('center_axis',(0.,1.,0.));
#3583=DIRECTION('ref_axis',(1.,0.,0.));
#3584=DIRECTION('center_axis',(-1.,0.,0.));
#3585=DIRECTION('ref_axis',(0.,0.,1.));
#3586=DIRECTION('',(0.,0.,1.));
#3587=DIRECTION('center_axis',(0.,1.,0.));
#3588=DIRECTION('ref_axis',(0.,0.,1.));
#3589=DIRECTION('center_axis',(1.,0.,0.));
#3590=DIRECTION('ref_axis',(0.,0.,-1.));
#3591=DIRECTION('center_axis',(1.,0.,0.));
#3592=DIRECTION('ref_axis',(0.,0.,-1.));
#3593=DIRECTION('',(-1.,0.,0.));
#3594=DIRECTION('center_axis',(1.,0.,0.));
#3595=DIRECTION('ref_axis',(0.,0.,-1.));
#3596=DIRECTION('axis',(0.,0.,1.));
#3597=DIRECTION('refdir',(1.,0.,0.));
#3598=DIRECTION('center_axis',(0.,-1.,0.));
#3599=DIRECTION('ref_axis',(1.,0.,0.));
#3600=DIRECTION('center_axis',(0.,1.,0.));
#3601=DIRECTION('ref_axis',(1.,0.,0.));
#3602=DIRECTION('',(0.,1.,0.));
#3603=DIRECTION('center_axis',(0.,-1.,0.));
#3604=DIRECTION('ref_axis',(1.,0.,0.));
#3605=DIRECTION('center_axis',(0.,1.,0.));
#3606=DIRECTION('ref_axis',(1.,0.,0.));
#3607=DIRECTION('center_axis',(0.,-1.,0.));
#3608=DIRECTION('ref_axis',(1.,0.,0.));
#3609=DIRECTION('',(-0.707106781186549,0.707106781186546,-8.65956056235496E-17));
#3610=DIRECTION('center_axis',(0.,-1.,0.));
#3611=DIRECTION('ref_axis',(0.,0.,-1.));
#3612=DIRECTION('center_axis',(0.,-1.,0.));
#3613=DIRECTION('ref_axis',(1.,0.,0.));
#3614=DIRECTION('center_axis',(0.,1.,0.));
#3615=DIRECTION('ref_axis',(1.,0.,0.));
#3616=DIRECTION('',(-0.866025403784439,-0.5,-1.06057523872491E-16));
#3617=DIRECTION('center_axis',(1.4792020664489E-16,0.,-1.));
#3618=DIRECTION('ref_axis',(-1.,0.,-1.4792020664489E-16));
#3619=DIRECTION('',(0.,1.,0.));
#3620=DIRECTION('',(-1.,0.,-1.4792020664489E-16));
#3621=DIRECTION('',(0.,1.,0.));
#3622=DIRECTION('center_axis',(0.866025403784439,0.,-0.5));
#3623=DIRECTION('ref_axis',(-0.5,0.,-0.866025403784439));
#3624=DIRECTION('',(0.,1.,0.));
#3625=DIRECTION('',(-0.5,0.,-0.866025403784439));
#3626=DIRECTION('center_axis',(0.866025403784439,0.,0.5));
#3627=DIRECTION('ref_axis',(0.5,0.,-0.866025403784439));
#3628=DIRECTION('',(0.,1.,0.));
#3629=DIRECTION('',(0.5,0.,-0.866025403784439));
#3630=DIRECTION('center_axis',(-2.95840413289779E-16,0.,1.));
#3631=DIRECTION('ref_axis',(1.,0.,2.95840413289779E-16));
#3632=DIRECTION('',(0.,1.,0.));
#3633=DIRECTION('',(1.,0.,2.95840413289779E-16));
#3634=DIRECTION('center_axis',(-0.866025403784439,0.,0.5));
#3635=DIRECTION('ref_axis',(0.5,0.,0.866025403784439));
#3636=DIRECTION('',(0.,1.,0.));
#3637=DIRECTION('',(0.5,0.,0.866025403784439));
#3638=DIRECTION('center_axis',(-0.866025403784439,0.,-0.5));
#3639=DIRECTION('ref_axis',(-0.5,0.,0.866025403784439));
#3640=DIRECTION('',(-0.5,0.,0.866025403784439));
#3641=DIRECTION('center_axis',(0.,1.,0.));
#3642=DIRECTION('ref_axis',(0.,0.,1.));
#3643=DIRECTION('center_axis',(0.,1.,0.));
#3644=DIRECTION('ref_axis',(1.,0.,0.));
#3645=DIRECTION('axis',(0.,0.,1.));
#3646=DIRECTION('refdir',(1.,0.,0.));
#3647=DIRECTION('center_axis',(0.,1.,0.));
#3648=DIRECTION('ref_axis',(1.,0.,0.));
#3649=DIRECTION('',(0.866025403784439,-0.5,1.06057523872491E-16));
#3650=DIRECTION('center_axis',(0.,-1.,0.));
#3651=DIRECTION('ref_axis',(1.,0.,0.));
#3652=DIRECTION('center_axis',(0.,-1.,0.));
#3653=DIRECTION('ref_axis',(1.,0.,0.));
#3654=DIRECTION('center_axis',(0.,1.,0.));
#3655=DIRECTION('ref_axis',(1.,0.,0.));
#3656=DIRECTION('',(-0.866025403784439,-0.5,-1.06057523872491E-16));
#3657=DIRECTION('center_axis',(1.4792020664489E-16,0.,-1.));
#3658=DIRECTION('ref_axis',(-1.,0.,-1.4792020664489E-16));
#3659=DIRECTION('',(0.,1.,0.));
#3660=DIRECTION('',(0.,1.,0.));
#3661=DIRECTION('center_axis',(-0.866025403784439,0.,-0.5));
#3662=DIRECTION('ref_axis',(-0.5,0.,0.866025403784439));
#3663=DIRECTION('',(0.,1.,0.));
#3664=DIRECTION('center_axis',(-0.866025403784439,0.,0.5));
#3665=DIRECTION('ref_axis',(0.5,0.,0.866025403784439));
#3666=DIRECTION('',(0.,1.,0.));
#3667=DIRECTION('center_axis',(0.,1.,0.));
#3668=DIRECTION('ref_axis',(1.,0.,0.));
#3669=DIRECTION('center_axis',(0.,1.,0.));
#3670=DIRECTION('ref_axis',(1.,0.,0.));
#3671=DIRECTION('',(0.,-1.,0.));
#3672=DIRECTION('center_axis',(0.,1.,0.));
#3673=DIRECTION('ref_axis',(1.,0.,0.));
#3674=DIRECTION('center_axis',(-2.95840413289779E-16,0.,1.));
#3675=DIRECTION('ref_axis',(1.,0.,2.95840413289779E-16));
#3676=DIRECTION('',(0.,1.,0.));
#3677=DIRECTION('center_axis',(0.866025403784439,0.,-0.5));
#3678=DIRECTION('ref_axis',(-0.5,0.,-0.866025403784439));
#3679=DIRECTION('',(0.,1.,0.));
#3680=DIRECTION('center_axis',(0.866025403784439,0.,0.5));
#3681=DIRECTION('ref_axis',(0.5,0.,-0.866025403784439));
#3682=DIRECTION('center_axis',(0.,1.,0.));
#3683=DIRECTION('ref_axis',(1.,0.,0.));
#3684=DIRECTION('center_axis',(0.,1.,0.));
#3685=DIRECTION('ref_axis',(1.,0.,0.));
#3686=DIRECTION('axis',(0.,0.,1.));
#3687=DIRECTION('refdir',(1.,0.,0.));
#3688=DIRECTION('center_axis',(0.,0.,1.));
#3689=DIRECTION('ref_axis',(1.,0.,0.));
#3690=DIRECTION('center_axis',(0.,0.,1.));
#3691=DIRECTION('ref_axis',(1.,0.,0.));
#3692=DIRECTION('',(0.,0.,-1.));
#3693=DIRECTION('center_axis',(0.,0.,1.));
#3694=DIRECTION('ref_axis',(1.,0.,0.));
#3695=DIRECTION('center_axis',(0.,0.,1.));
#3696=DIRECTION('ref_axis',(1.,0.,0.));
#3697=DIRECTION('center_axis',(0.,0.,1.));
#3698=DIRECTION('ref_axis',(1.,0.,0.));
#3699=DIRECTION('axis',(0.,0.,1.));
#3700=DIRECTION('refdir',(1.,0.,0.));
#3701=DIRECTION('center_axis',(1.,0.,0.));
#3702=DIRECTION('ref_axis',(0.,0.,-1.));
#3703=DIRECTION('',(1.,0.,0.));
#3704=DIRECTION('center_axis',(0.,1.,0.));
#3705=DIRECTION('ref_axis',(0.,0.,1.));
#3706=DIRECTION('center_axis',(0.,-1.,0.));
#3707=DIRECTION('ref_axis',(1.,0.,0.));
#3708=DIRECTION('center_axis',(0.,-1.,0.));
#3709=DIRECTION('ref_axis',(1.,0.,0.));
#3710=DIRECTION('center_axis',(0.,-1.,0.));
#3711=DIRECTION('ref_axis',(1.,0.,0.));
#3712=DIRECTION('',(0.707106781186547,0.707106781186548,8.65956056235493E-17));
#3713=DIRECTION('center_axis',(0.,-1.,0.));
#3714=DIRECTION('ref_axis',(1.,0.,0.));
#3715=DIRECTION('center_axis',(0.,-1.,0.));
#3716=DIRECTION('ref_axis',(1.,0.,0.));
#3717=DIRECTION('',(0.,1.,0.));
#3718=DIRECTION('center_axis',(0.,-1.,0.));
#3719=DIRECTION('ref_axis',(0.,0.,-1.));
#3720=DIRECTION('center_axis',(0.,-1.,0.));
#3721=DIRECTION('ref_axis',(1.,0.,0.));
#3722=DIRECTION('center_axis',(0.,-1.,0.));
#3723=DIRECTION('ref_axis',(1.,0.,0.));
#3724=DIRECTION('center_axis',(0.,-1.,0.));
#3725=DIRECTION('ref_axis',(1.,0.,0.));
#3726=DIRECTION('',(0.,1.,0.));
#3727=DIRECTION('',(0.,1.,0.));
#3728=DIRECTION('center_axis',(0.,1.,0.));
#3729=DIRECTION('ref_axis',(1.,0.,0.));
#3730=DIRECTION('center_axis',(0.,-1.,0.));
#3731=DIRECTION('ref_axis',(1.,0.,0.));
#3732=DIRECTION('',(-0.707106781186548,0.707106781186547,-8.65956056235494E-17));
#3733=DIRECTION('center_axis',(0.,-1.,0.));
#3734=DIRECTION('ref_axis',(0.,0.,-1.));
#3735=DIRECTION('axis',(0.,0.,1.));
#3736=DIRECTION('refdir',(1.,0.,0.));
#3737=DIRECTION('center_axis',(0.,1.,0.));
#3738=DIRECTION('ref_axis',(1.,0.,0.));
#3739=DIRECTION('center_axis',(0.,-1.,0.));
#3740=DIRECTION('ref_axis',(1.,0.,0.));
#3741=DIRECTION('',(0.,-1.,0.));
#3742=DIRECTION('center_axis',(0.,-1.,0.));
#3743=DIRECTION('ref_axis',(1.,0.,0.));
#3744=DIRECTION('center_axis',(0.,1.,0.));
#3745=DIRECTION('ref_axis',(1.,0.,0.));
#3746=DIRECTION('center_axis',(0.,1.,0.));
#3747=DIRECTION('ref_axis',(1.,0.,0.));
#3748=DIRECTION('',(0.,-1.,0.));
#3749=DIRECTION('center_axis',(0.,1.,0.));
#3750=DIRECTION('ref_axis',(1.,0.,0.));
#3751=DIRECTION('center_axis',(0.,1.,0.));
#3752=DIRECTION('ref_axis',(1.,0.,0.));
#3753=DIRECTION('center_axis',(0.,1.,0.));
#3754=DIRECTION('ref_axis',(1.,0.,0.));
#3755=DIRECTION('axis',(0.,0.,1.));
#3756=DIRECTION('refdir',(1.,0.,0.));
#3757=DIRECTION('center_axis',(0.,1.,0.));
#3758=DIRECTION('ref_axis',(1.,0.,0.));
#3759=DIRECTION('center_axis',(0.,-1.,0.));
#3760=DIRECTION('ref_axis',(1.,0.,0.));
#3761=DIRECTION('',(0.,-1.,0.));
#3762=DIRECTION('center_axis',(0.,-1.,0.));
#3763=DIRECTION('ref_axis',(1.,0.,0.));
#3764=DIRECTION('center_axis',(0.,1.,0.));
#3765=DIRECTION('ref_axis',(1.,0.,0.));
#3766=DIRECTION('center_axis',(0.,1.,0.));
#3767=DIRECTION('ref_axis',(1.,0.,0.));
#3768=DIRECTION('',(0.,-1.,0.));
#3769=DIRECTION('center_axis',(0.,1.,0.));
#3770=DIRECTION('ref_axis',(1.,0.,0.));
#3771=DIRECTION('center_axis',(0.,1.,0.));
#3772=DIRECTION('ref_axis',(1.,0.,0.));
#3773=DIRECTION('center_axis',(0.,1.,0.));
#3774=DIRECTION('ref_axis',(1.,0.,0.));
#3775=DIRECTION('axis',(0.,0.,1.));
#3776=DIRECTION('refdir',(1.,0.,0.));
#3777=DIRECTION('center_axis',(-1.,0.,0.));
#3778=DIRECTION('ref_axis',(0.,0.,1.));
#3779=DIRECTION('center_axis',(0.,-1.,1.38777878078145E-16));
#3780=DIRECTION('ref_axis',(0.,-1.38777878078145E-16,-1.));
#3781=DIRECTION('center_axis',(1.,0.,0.));
#3782=DIRECTION('ref_axis',(0.,0.,1.));
#3783=DIRECTION('center_axis',(0.,1.,0.));
#3784=DIRECTION('ref_axis',(1.,0.,0.));
#3785=DIRECTION('center_axis',(0.,-1.,0.));
#3786=DIRECTION('ref_axis',(1.,0.,0.));
#3787=DIRECTION('',(0.,0.,1.));
#3788=DIRECTION('center_axis',(1.,0.,0.));
#3789=DIRECTION('ref_axis',(0.,0.,1.));
#3790=DIRECTION('',(0.,-1.,0.));
#3791=DIRECTION('',(0.,0.,1.));
#3792=DIRECTION('',(0.,-1.,0.));
#3793=DIRECTION('center_axis',(0.,-1.,0.));
#3794=DIRECTION('ref_axis',(1.,0.,0.));
#3795=DIRECTION('center_axis',(0.,-1.,0.));
#3796=DIRECTION('ref_axis',(1.,0.,0.));
#3797=DIRECTION('',(0.,1.,0.));
#3798=DIRECTION('center_axis',(0.,-1.,0.));
#3799=DIRECTION('ref_axis',(1.,0.,0.));
#3800=DIRECTION('center_axis',(0.,1.,0.));
#3801=DIRECTION('ref_axis',(1.,0.,0.));
#3802=DIRECTION('',(0.,0.,1.));
#3803=DIRECTION('',(1.,0.,0.));
#3804=DIRECTION('',(0.,0.,1.));
#3805=DIRECTION('',(1.,0.,0.));
#3806=DIRECTION('',(0.,0.,1.));
#3807=DIRECTION('',(1.,0.,0.));
#3808=DIRECTION('',(0.,0.,1.));
#3809=DIRECTION('',(1.,0.,0.));
#3810=DIRECTION('',(0.,0.,1.));
#3811=DIRECTION('',(1.,0.,0.));
#3812=DIRECTION('',(0.,0.,1.));
#3813=DIRECTION('',(2.22044604925031E-16,1.,0.));
#3814=DIRECTION('',(0.,0.,1.));
#3815=DIRECTION('',(1.,0.,0.));
#3816=DIRECTION('',(0.,0.,1.));
#3817=DIRECTION('',(1.,0.,0.));
#3818=DIRECTION('',(0.,0.,1.));
#3819=DIRECTION('',(1.,0.,0.));
#3820=DIRECTION('',(0.,0.,1.));
#3821=DIRECTION('',(1.,0.,0.));
#3822=DIRECTION('',(0.,0.,1.));
#3823=DIRECTION('',(1.,0.,0.));
#3824=DIRECTION('',(0.,0.,1.));
#3825=DIRECTION('',(1.,0.,0.));
#3826=DIRECTION('',(0.,0.,1.));
#3827=DIRECTION('',(1.,0.,0.));
#3828=DIRECTION('',(0.,0.,1.));
#3829=DIRECTION('',(2.22044604925031E-16,1.,0.));
#3830=DIRECTION('',(0.,0.,1.));
#3831=DIRECTION('',(1.,0.,0.));
#3832=DIRECTION('',(0.,0.,1.));
#3833=DIRECTION('',(2.22044604925031E-16,-1.,0.));
#3834=DIRECTION('',(0.,0.,1.));
#3835=DIRECTION('',(2.22044604925031E-16,-1.,0.));
#3836=DIRECTION('',(1.,0.,2.22044604925031E-16));
#3837=DIRECTION('',(2.22044604925031E-16,0.,-1.));
#3838=DIRECTION('',(0.,0.,1.));
#3839=DIRECTION('',(1.,0.,0.));
#3840=DIRECTION('',(0.,0.,1.));
#3841=DIRECTION('',(1.,0.,0.));
#3842=DIRECTION('',(0.,0.,1.));
#3843=DIRECTION('',(1.,0.,0.));
#3844=DIRECTION('',(0.,0.,1.));
#3845=DIRECTION('',(1.,0.,0.));
#3846=DIRECTION('',(0.,0.,1.));
#3847=DIRECTION('',(2.22044604925031E-16,1.,0.));
#3848=DIRECTION('',(0.,0.,1.));
#3849=DIRECTION('',(1.,0.,0.));
#3850=DIRECTION('',(0.,0.,1.));
#3851=DIRECTION('',(1.,0.,0.));
#3852=DIRECTION('',(0.,0.,1.));
#3853=DIRECTION('',(1.,0.,0.));
#3854=DIRECTION('',(0.,0.,1.));
#3855=DIRECTION('',(1.,0.,0.));
#3856=CARTESIAN_POINT('',(0.,0.,0.));
#3857=CARTESIAN_POINT('',(0.,0.,0.));
#3858=CARTESIAN_POINT('',(0.,0.,0.));
#3859=CARTESIAN_POINT('Origin',(1.04595925965485,-0.4,6.42376977244362));
#3860=CARTESIAN_POINT('',(1.04595925965485,0.9,6.12376977244362));
#3861=CARTESIAN_POINT('',(1.04595925965485,1.25,6.12376977244362));
#3862=CARTESIAN_POINT('',(1.04595925965485,0.9,6.12376977244362));
#3863=CARTESIAN_POINT('',(1.04595925965485,0.9,6.72376977244362));
#3864=CARTESIAN_POINT('Origin',(1.04595925965485,0.9,6.42376977244362));
#3865=CARTESIAN_POINT('',(1.04595925965485,1.25,6.72376977244362));
#3866=CARTESIAN_POINT('',(1.04595925965485,0.9,6.72376977244362));
#3867=CARTESIAN_POINT('',(0.745959259654855,1.25,6.42376977244362));
#3868=CARTESIAN_POINT('Origin',(1.04595925965485,1.25,6.42376977244362));
#3869=CARTESIAN_POINT('',(0.745959259654855,-0.4,6.42376977244362));
#3870=CARTESIAN_POINT('',(0.745959259654855,-0.4,6.42376977244362));
#3871=CARTESIAN_POINT('Origin',(1.04595925965485,-0.4,6.42376977244362));
#3872=CARTESIAN_POINT('Origin',(1.04595925965485,1.25,6.42376977244362));
#3873=CARTESIAN_POINT('Origin',(1.04595925965485,-0.4,6.42376977244362));
#3874=CARTESIAN_POINT('Origin',(11.,1.25,0.));
#3875=CARTESIAN_POINT('',(7.4,1.25,6.72376977244362));
#3876=CARTESIAN_POINT('',(7.4,1.25,6.72376977244362));
#3877=CARTESIAN_POINT('',(7.4,1.25,0.6));
#3878=CARTESIAN_POINT('',(7.4,1.25,6.12376977244362));
#3879=CARTESIAN_POINT('',(11.,1.25,0.6));
#3880=CARTESIAN_POINT('',(11.,1.25,0.6));
#3881=CARTESIAN_POINT('',(11.,1.25,0.));
#3882=CARTESIAN_POINT('',(11.,1.25,0.));
#3883=CARTESIAN_POINT('',(-2.,1.25,0.));
#3884=CARTESIAN_POINT('',(11.,1.25,0.));
#3885=CARTESIAN_POINT('',(-2.,1.25,0.6));
#3886=CARTESIAN_POINT('',(-2.,1.25,0.));
#3887=CARTESIAN_POINT('',(6.8,1.25,0.6));
#3888=CARTESIAN_POINT('',(11.,1.25,0.6));
#3889=CARTESIAN_POINT('',(6.8,1.25,6.12376977244362));
#3890=CARTESIAN_POINT('',(6.8,1.25,6.42376977244362));
#3891=CARTESIAN_POINT('',(1.04595925965485,1.25,6.12376977244362));
#3892=CARTESIAN_POINT('Origin',(7.4,0.9,6.12376977244362));
#3893=CARTESIAN_POINT('',(6.8,0.9,6.12376977244362));
#3894=CARTESIAN_POINT('',(6.8,0.9,6.12376977244362));
#3895=CARTESIAN_POINT('',(1.04595925965485,0.9,6.12376977244362));
#3896=CARTESIAN_POINT('Origin',(1.04595925965485,0.9,6.72376977244362));
#3897=CARTESIAN_POINT('',(7.4,0.9,6.72376977244362));
#3898=CARTESIAN_POINT('',(7.4,0.9,6.72376977244362));
#3899=CARTESIAN_POINT('',(7.4,0.9,6.72376977244362));
#3900=CARTESIAN_POINT('Origin',(7.4,0.9,6.42376977244362));
#3901=CARTESIAN_POINT('',(7.4,0.9,0.6));
#3902=CARTESIAN_POINT('',(7.4,0.9,6.12376977244362));
#3903=CARTESIAN_POINT('',(7.4,0.45,0.6));
#3904=CARTESIAN_POINT('Origin',(6.8,0.9,0.5));
#3905=CARTESIAN_POINT('',(6.8,0.9,0.6));
#3906=CARTESIAN_POINT('',(6.8,0.45,0.6));
#3907=CARTESIAN_POINT('',(6.8,0.9,6.42376977244362));
#3908=CARTESIAN_POINT('Origin',(7.1,0.9,3.46188488622181));
#3909=CARTESIAN_POINT('',(5.8,0.9,0.6));
#3910=CARTESIAN_POINT('Origin',(4.5,0.,0.6));
#3911=CARTESIAN_POINT('',(-2.,-1.25,0.6));
#3912=CARTESIAN_POINT('',(-2.,1.25,0.6));
#3913=CARTESIAN_POINT('',(11.,-1.25,0.6));
#3914=CARTESIAN_POINT('',(-2.,-1.25,0.6));
#3915=CARTESIAN_POINT('',(11.,-1.25,0.6));
#3916=CARTESIAN_POINT('',(0.7,-0.5,0.6));
#3917=CARTESIAN_POINT('',(0.7,-0.9,0.6));
#3918=CARTESIAN_POINT('',(0.7,-0.45,0.6));
#3919=CARTESIAN_POINT('',(-0.7,-0.9,0.6));
#3920=CARTESIAN_POINT('',(2.25,-0.9,0.6));
#3921=CARTESIAN_POINT('',(-0.7,-0.5,0.6));
#3922=CARTESIAN_POINT('',(-0.7,-0.45,0.6));
#3923=CARTESIAN_POINT('',(2.25,-0.5,0.6));
#3924=CARTESIAN_POINT('',(0.7,0.9,0.6));
#3925=CARTESIAN_POINT('',(0.7,0.5,0.6));
#3926=CARTESIAN_POINT('',(0.7,0.25,0.6));
#3927=CARTESIAN_POINT('',(-0.7,0.5,0.6));
#3928=CARTESIAN_POINT('',(2.25,0.5,0.6));
#3929=CARTESIAN_POINT('',(-0.7,0.9,0.6));
#3930=CARTESIAN_POINT('',(-0.7,0.25,0.6));
#3931=CARTESIAN_POINT('',(2.25,0.9,0.6));
#3932=CARTESIAN_POINT('',(10.,0.9,0.6));
#3933=CARTESIAN_POINT('',(10.,-0.9,0.6));
#3934=CARTESIAN_POINT('',(10.,-0.45,0.6));
#3935=CARTESIAN_POINT('',(8.5,-0.9,0.6));
#3936=CARTESIAN_POINT('',(6.875,-0.9,0.6));
#3937=CARTESIAN_POINT('',(8.5,0.9,0.6));
#3938=CARTESIAN_POINT('',(8.5,-0.45,0.6));
#3939=CARTESIAN_POINT('',(6.875,0.9,0.6));
#3940=CARTESIAN_POINT('',(10.225,3.36777869765523E-17,0.6));
#3941=CARTESIAN_POINT('Origin',(10.5,0.,0.6));
#3942=CARTESIAN_POINT('',(-1.475,3.36777869765522E-17,0.6));
#3943=CARTESIAN_POINT('Origin',(-1.2,0.,0.6));
#3944=CARTESIAN_POINT('Origin',(-1.2,0.,-0.1));
#3945=CARTESIAN_POINT('',(-1.475,-3.36777869765522E-17,0.));
#3946=CARTESIAN_POINT('Origin',(-1.2,0.,0.));
#3947=CARTESIAN_POINT('',(-1.475,-3.36777869765522E-17,-0.1));
#3948=CARTESIAN_POINT('Origin',(10.5,0.,-0.1));
#3949=CARTESIAN_POINT('',(10.225,-3.36777869765523E-17,0.));
#3950=CARTESIAN_POINT('Origin',(10.5,0.,0.));
#3951=CARTESIAN_POINT('',(10.225,-3.36777869765523E-17,-0.1));
#3952=CARTESIAN_POINT('Origin',(8.4,0.,2.5));
#3953=CARTESIAN_POINT('',(8.5,-6.2456986756515E-17,3.01));
#3954=CARTESIAN_POINT('Origin',(8.5,0.,2.5));
#3955=CARTESIAN_POINT('',(10.,6.2456986756515E-17,3.01));
#3956=CARTESIAN_POINT('',(8.4,-6.2456986756515E-17,3.01));
#3957=CARTESIAN_POINT('Origin',(10.,0.,2.5));
#3958=CARTESIAN_POINT('Origin',(9.25,-0.9,2.));
#3959=CARTESIAN_POINT('',(10.,-0.9,3.5));
#3960=CARTESIAN_POINT('',(10.,-0.9,0.5));
#3961=CARTESIAN_POINT('',(8.5,-0.9,3.5));
#3962=CARTESIAN_POINT('',(10.,-0.9,3.5));
#3963=CARTESIAN_POINT('',(8.5,-0.9,3.5));
#3964=CARTESIAN_POINT('Origin',(10.,-0.9,3.5));
#3965=CARTESIAN_POINT('',(10.,0.9,3.5));
#3966=CARTESIAN_POINT('',(10.,0.9,0.5));
#3967=CARTESIAN_POINT('',(10.,-0.9,3.5));
#3968=CARTESIAN_POINT('Origin',(8.5,-0.9,0.5));
#3969=CARTESIAN_POINT('',(8.5,0.9,3.5));
#3970=CARTESIAN_POINT('',(8.5,-0.9,3.5));
#3971=CARTESIAN_POINT('',(8.5,0.9,3.5));
#3972=CARTESIAN_POINT('Origin',(8.5,-0.9,3.5));
#3973=CARTESIAN_POINT('',(10.,0.9,3.5));
#3974=CARTESIAN_POINT('Origin',(9.25,0.9,2.));
#3975=CARTESIAN_POINT('Origin',(0.,-1.,2.5));
#3976=CARTESIAN_POINT('',(-0.31,-0.9,2.5));
#3977=CARTESIAN_POINT('Origin',(0.,-0.9,2.5));
#3978=CARTESIAN_POINT('',(-0.31,-0.5,2.5));
#3979=CARTESIAN_POINT('',(-0.31,-1.,2.5));
#3980=CARTESIAN_POINT('Origin',(0.,-0.5,2.5));
#3981=CARTESIAN_POINT('Origin',(0.,-1.,2.5));
#3982=CARTESIAN_POINT('',(-0.31,0.5,2.5));
#3983=CARTESIAN_POINT('Origin',(0.,0.5,2.5));
#3984=CARTESIAN_POINT('',(-0.31,0.9,2.5));
#3985=CARTESIAN_POINT('',(-0.31,-1.,2.5));
#3986=CARTESIAN_POINT('Origin',(0.,0.9,2.5));
#3987=CARTESIAN_POINT('Origin',(0.,0.5,1.9));
#3988=CARTESIAN_POINT('',(0.7,0.5,3.3));
#3989=CARTESIAN_POINT('',(0.7,0.5,0.5));
#3990=CARTESIAN_POINT('',(-0.7,0.5,3.3));
#3991=CARTESIAN_POINT('',(0.7,0.5,3.3));
#3992=CARTESIAN_POINT('',(-0.7,0.5,3.3));
#3993=CARTESIAN_POINT('Origin',(0.7,0.5,3.3));
#3994=CARTESIAN_POINT('',(0.7,0.9,3.3));
#3995=CARTESIAN_POINT('',(0.7,0.9,0.5));
#3996=CARTESIAN_POINT('',(0.7,0.5,3.3));
#3997=CARTESIAN_POINT('Origin',(-0.7,0.5,0.5));
#3998=CARTESIAN_POINT('',(-0.7,0.9,3.3));
#3999=CARTESIAN_POINT('',(-0.7,0.5,3.3));
#4000=CARTESIAN_POINT('',(-0.7,0.9,3.3));
#4001=CARTESIAN_POINT('Origin',(-0.7,0.5,3.3));
#4002=CARTESIAN_POINT('',(0.7,0.9,3.3));
#4003=CARTESIAN_POINT('Origin',(0.,0.9,1.9));
#4004=CARTESIAN_POINT('Origin',(0.,-0.9,1.9));
#4005=CARTESIAN_POINT('',(0.7,-0.9,3.3));
#4006=CARTESIAN_POINT('',(0.7,-0.9,0.5));
#4007=CARTESIAN_POINT('',(-0.7,-0.9,3.3));
#4008=CARTESIAN_POINT('',(0.7,-0.9,3.3));
#4009=CARTESIAN_POINT('',(-0.7,-0.9,3.3));
#4010=CARTESIAN_POINT('Origin',(0.7,-0.9,3.3));
#4011=CARTESIAN_POINT('',(0.7,-0.5,3.3));
#4012=CARTESIAN_POINT('',(0.7,-0.5,0.5));
#4013=CARTESIAN_POINT('',(0.7,-0.9,3.3));
#4014=CARTESIAN_POINT('Origin',(-0.7,-0.9,0.5));
#4015=CARTESIAN_POINT('',(-0.7,-0.5,3.3));
#4016=CARTESIAN_POINT('',(-0.7,-0.9,3.3));
#4017=CARTESIAN_POINT('',(-0.7,-0.5,3.3));
#4018=CARTESIAN_POINT('Origin',(-0.7,-0.9,3.3));
#4019=CARTESIAN_POINT('',(0.7,-0.5,3.3));
#4020=CARTESIAN_POINT('Origin',(0.,-0.5,1.9));
#4021=CARTESIAN_POINT('Origin',(11.,-1.25,0.));
#4022=CARTESIAN_POINT('',(11.,-1.25,0.));
#4023=CARTESIAN_POINT('',(11.,-1.25,0.));
#4024=CARTESIAN_POINT('',(11.,-1.25,0.));
#4025=CARTESIAN_POINT('Origin',(-2.,-1.25,0.));
#4026=CARTESIAN_POINT('',(-2.,-1.25,0.));
#4027=CARTESIAN_POINT('',(-2.,-1.25,0.));
#4028=CARTESIAN_POINT('',(-2.,-1.25,0.));
#4029=CARTESIAN_POINT('Origin',(-2.,1.25,0.));
#4030=CARTESIAN_POINT('',(-2.,1.25,0.));
#4031=CARTESIAN_POINT('Origin',(4.5,0.,0.));
#4032=CARTESIAN_POINT('',(0.,0.,0.));
#4033=CARTESIAN_POINT('',(0.,0.,0.));
#4034=CARTESIAN_POINT('Origin',(0.435778713738291,-0.4,7.48097349045873));
#4035=CARTESIAN_POINT('',(0.160778713738291,-0.3,7.48097349045873));
#4036=CARTESIAN_POINT('Origin',(0.435778713738291,-0.3,7.48097349045873));
#4037=CARTESIAN_POINT('',(0.160778713738291,0.3,7.48097349045873));
#4038=CARTESIAN_POINT('',(0.160778713738291,-0.4,7.48097349045873));
#4039=CARTESIAN_POINT('Origin',(0.435778713738291,0.3,7.48097349045873));
#4040=CARTESIAN_POINT('Origin',(0.,-0.6,2.5));
#4041=CARTESIAN_POINT('',(-0.31,-0.48,2.5));
#4042=CARTESIAN_POINT('Origin',(0.,-0.48,2.5));
#4043=CARTESIAN_POINT('',(-0.31,0.48,2.5));
#4044=CARTESIAN_POINT('',(-0.31,-0.6,2.5));
#4045=CARTESIAN_POINT('Origin',(0.,0.48,2.5));
#4046=CARTESIAN_POINT('Origin',(0.435778713738291,-0.3,7.48097349045873));
#4047=CARTESIAN_POINT('',(0.784189430553042,0.3,6.87384090822596));
#4048=CARTESIAN_POINT('',(0.784189430553042,-0.3,6.87384090822596));
#4049=CARTESIAN_POINT('',(0.784189430553042,-0.3,6.87384090822596));
#4050=CARTESIAN_POINT('',(-0.0127663279203548,0.3,6.94356550242408));
#4051=CARTESIAN_POINT('Origin',(0.435778713738291,0.3,7.48097349045873));
#4052=CARTESIAN_POINT('',(-0.0127663279203548,-0.3,6.94356550242408));
#4053=CARTESIAN_POINT('',(-0.0127663279203548,-0.3,6.94356550242408));
#4054=CARTESIAN_POINT('Origin',(0.435778713738291,-0.3,7.48097349045873));
#4055=CARTESIAN_POINT('Origin',(0.217889356869145,-0.3,4.99048674522937));
#4056=CARTESIAN_POINT('',(-0.359500646154049,-0.3,2.98037410985067));
#4057=CARTESIAN_POINT('',(-0.398477879236698,-0.3,2.53486229709906));
#4058=CARTESIAN_POINT('',(0.437455112319348,-0.3,2.91064951565254));
#4059=CARTESIAN_POINT('Origin',(0.,-0.3,2.5));
#4060=CARTESIAN_POINT('',(0.834256592974989,-0.3,7.44611119335967));
#4061=CARTESIAN_POINT('Origin',(-0.398477879236698,-0.3,2.53486229709906));
#4062=CARTESIAN_POINT('',(-0.359500646154049,0.3,2.98037410985067));
#4063=CARTESIAN_POINT('',(-0.398477879236698,0.3,2.53486229709906));
#4064=CARTESIAN_POINT('',(-0.359500646154049,-0.48,2.98037410985067));
#4065=CARTESIAN_POINT('Origin',(0.217889356869145,0.3,4.99048674522937));
#4066=CARTESIAN_POINT('',(0.437455112319348,0.3,2.91064951565254));
#4067=CARTESIAN_POINT('',(0.834256592974989,0.3,7.44611119335967));
#4068=CARTESIAN_POINT('Origin',(0.,0.3,2.5));
#4069=CARTESIAN_POINT('Origin',(0.834256592974989,-0.3,7.44611119335967));
#4070=CARTESIAN_POINT('',(0.437455112319348,-0.48,2.91064951565254));
#4071=CARTESIAN_POINT('Origin',(2.49048674522936,-1.,2.28211064313085));
#4072=CARTESIAN_POINT('',(2.18048674522936,-0.9,2.28211064313085));
#4073=CARTESIAN_POINT('Origin',(2.49048674522936,-0.9,2.28211064313085));
#4074=CARTESIAN_POINT('',(2.18048674522936,-0.5,2.28211064313085));
#4075=CARTESIAN_POINT('',(2.18048674522936,-1.,2.28211064313085));
#4076=CARTESIAN_POINT('Origin',(2.49048674522936,-0.5,2.28211064313085));
#4077=CARTESIAN_POINT('Origin',(2.49048674522936,-1.,2.28211064313085));
#4078=CARTESIAN_POINT('',(2.18048674522936,0.5,2.28211064313085));
#4079=CARTESIAN_POINT('Origin',(2.49048674522936,0.5,2.28211064313085));
#4080=CARTESIAN_POINT('',(2.18048674522936,0.9,2.28211064313085));
#4081=CARTESIAN_POINT('',(2.18048674522936,-1.,2.28211064313085));
#4082=CARTESIAN_POINT('Origin',(2.49048674522936,0.9,2.28211064313085));
#4083=CARTESIAN_POINT('Origin',(1.66363611114492,-0.9,3.15750657007714));
#4084=CARTESIAN_POINT('',(1.52418692274867,-0.5,1.56359505313035));
#4085=CARTESIAN_POINT('',(1.66363611114492,-0.5,3.15750657007714));
#4086=CARTESIAN_POINT('',(1.62877381404586,-0.5,2.75902869084045));
#4087=CARTESIAN_POINT('',(1.52418692274867,0.5,1.56359505313035));
#4088=CARTESIAN_POINT('',(1.52418692274867,-0.9,1.56359505313035));
#4089=CARTESIAN_POINT('',(1.66363611114492,0.5,3.15750657007714));
#4090=CARTESIAN_POINT('',(1.62877381404586,0.5,2.75902869084045));
#4091=CARTESIAN_POINT('',(1.66363611114492,-0.9,3.15750657007714));
#4092=CARTESIAN_POINT('Origin',(2.29124780561101,0.9,2.29954179168039));
#4093=CARTESIAN_POINT('',(1.3647777017174,0.9,3.18365329290144));
#4094=CARTESIAN_POINT('',(3.35716709790089,0.9,3.00934180740612));
#4095=CARTESIAN_POINT('',(3.35716709790089,0.9,3.00934180740612));
#4096=CARTESIAN_POINT('',(3.21771790950463,0.9,1.41543029045933));
#4097=CARTESIAN_POINT('',(3.21771790950463,0.9,1.41543029045933));
#4098=CARTESIAN_POINT('',(1.22532851332114,0.9,1.58974177595465));
#4099=CARTESIAN_POINT('',(1.22532851332114,0.9,1.58974177595465));
#4100=CARTESIAN_POINT('',(1.3647777017174,0.9,3.18365329290144));
#4101=CARTESIAN_POINT('Origin',(3.35716709790089,0.5,3.00934180740612));
#4102=CARTESIAN_POINT('',(3.21771790950463,0.5,1.41543029045933));
#4103=CARTESIAN_POINT('',(3.35716709790089,0.5,3.00934180740612));
#4104=CARTESIAN_POINT('',(3.21771790950463,0.5,1.41543029045933));
#4105=CARTESIAN_POINT('',(3.21771790950463,0.5,1.41543029045933));
#4106=CARTESIAN_POINT('',(3.35716709790089,0.5,3.00934180740612));
#4107=CARTESIAN_POINT('Origin',(2.29124780561101,0.5,2.29954179168039));
#4108=CARTESIAN_POINT('',(1.22532851332114,0.5,1.58974177595465));
#4109=CARTESIAN_POINT('',(3.35716709790089,0.5,3.00934180740612));
#4110=CARTESIAN_POINT('Origin',(0.747146023568809,-0.3,2.43463319293926));
#4111=CARTESIAN_POINT('',(1.26019081042021,-0.3,1.98821965519135));
#4112=CARTESIAN_POINT('',(1.32991540461833,-0.3,2.78517541366474));
#4113=CARTESIAN_POINT('',(1.26019081042021,-0.3,1.98821965519135));
#4114=CARTESIAN_POINT('',(0.480374109850668,-0.3,2.85950064615405));
#4115=CARTESIAN_POINT('',(0.0348622970990633,-0.3,2.8984778792367));
#4116=CARTESIAN_POINT('',(0.410649515652541,-0.3,2.06254488768065));
#4117=CARTESIAN_POINT('Origin',(0.,-0.3,2.5));
#4118=CARTESIAN_POINT('',(1.45942975003856,-0.3,1.97078850664181));
#4119=CARTESIAN_POINT('Origin',(0.0348622970990633,-0.3,2.8984778792367));
#4120=CARTESIAN_POINT('',(1.32991540461833,0.3,2.78517541366474));
#4121=CARTESIAN_POINT('',(1.32991540461833,-0.6,2.78517541366474));
#4122=CARTESIAN_POINT('',(0.480374109850668,0.3,2.85950064615405));
#4123=CARTESIAN_POINT('',(0.0348622970990633,0.3,2.8984778792367));
#4124=CARTESIAN_POINT('',(0.480374109850668,-0.48,2.85950064615405));
#4125=CARTESIAN_POINT('Origin',(0.747146023568809,0.3,2.43463319293926));
#4126=CARTESIAN_POINT('',(1.26019081042021,0.3,1.98821965519135));
#4127=CARTESIAN_POINT('',(1.26019081042021,0.3,1.98821965519135));
#4128=CARTESIAN_POINT('',(0.410649515652541,0.3,2.06254488768065));
#4129=CARTESIAN_POINT('',(1.45942975003856,0.3,1.97078850664181));
#4130=CARTESIAN_POINT('Origin',(0.,0.3,2.5));
#4131=CARTESIAN_POINT('Origin',(1.45942975003856,-0.3,1.97078850664181));
#4132=CARTESIAN_POINT('',(1.26019081042021,-0.6,1.98821965519135));
#4133=CARTESIAN_POINT('',(0.410649515652541,-0.48,2.06254488768065));
#4134=CARTESIAN_POINT('Origin',(0.,-0.48,2.5));
#4135=CARTESIAN_POINT('',(-0.6,0.48,2.5));
#4136=CARTESIAN_POINT('Origin',(0.,0.48,2.5));
#4137=CARTESIAN_POINT('',(-0.6,-0.48,2.5));
#4138=CARTESIAN_POINT('',(-0.6,-0.48,2.5));
#4139=CARTESIAN_POINT('Origin',(0.,-0.48,2.5));
#4140=CARTESIAN_POINT('Origin',(0.,0.48,2.5));
#4141=CARTESIAN_POINT('Origin',(0.,-0.48,2.5));
#4142=CARTESIAN_POINT('Origin',(3.21771790950463,-0.9,1.41543029045933));
#4143=CARTESIAN_POINT('',(3.21771790950463,-0.5,1.41543029045933));
#4144=CARTESIAN_POINT('',(1.22532851332114,-0.5,1.58974177595465));
#4145=CARTESIAN_POINT('',(3.21771790950463,-0.9,1.41543029045933));
#4146=CARTESIAN_POINT('',(3.21771790950463,-0.9,1.41543029045933));
#4147=CARTESIAN_POINT('',(1.22532851332114,-0.9,1.58974177595465));
#4148=CARTESIAN_POINT('',(1.22532851332114,-0.9,1.58974177595465));
#4149=CARTESIAN_POINT('',(1.22532851332114,-0.9,1.58974177595465));
#4150=CARTESIAN_POINT('Origin',(2.29124780561101,-0.5,2.29954179168039));
#4151=CARTESIAN_POINT('',(3.35716709790089,-0.5,3.00934180740612));
#4152=CARTESIAN_POINT('',(3.35716709790089,-0.5,3.00934180740612));
#4153=CARTESIAN_POINT('',(3.21771790950463,-0.5,1.41543029045933));
#4154=CARTESIAN_POINT('Origin',(1.22532851332114,-0.9,1.58974177595465));
#4155=CARTESIAN_POINT('',(1.3647777017174,-0.9,3.18365329290144));
#4156=CARTESIAN_POINT('',(1.3647777017174,-0.9,3.18365329290144));
#4157=CARTESIAN_POINT('',(1.3647777017174,-0.9,3.18365329290144));
#4158=CARTESIAN_POINT('Origin',(3.35716709790089,-0.9,3.00934180740612));
#4159=CARTESIAN_POINT('',(3.35716709790089,-0.9,3.00934180740612));
#4160=CARTESIAN_POINT('',(3.21771790950463,-0.9,1.41543029045933));
#4161=CARTESIAN_POINT('',(3.35716709790089,-0.9,3.00934180740612));
#4162=CARTESIAN_POINT('Origin',(1.3647777017174,-0.9,3.18365329290144));
#4163=CARTESIAN_POINT('',(3.35716709790089,-0.9,3.00934180740612));
#4164=CARTESIAN_POINT('Origin',(2.29124780561101,-0.9,2.29954179168039));
#4165=CARTESIAN_POINT('',(0.,0.,0.));
#4166=CARTESIAN_POINT('Origin',(0.,-7.7,10.03));
#4167=CARTESIAN_POINT('',(-0.21,-7.7,10.03));
#4168=CARTESIAN_POINT('Origin',(0.,-7.7,10.03));
#4169=CARTESIAN_POINT('',(-0.21,-6.5,10.03));
#4170=CARTESIAN_POINT('',(-0.21,-7.7,10.03));
#4171=CARTESIAN_POINT('Origin',(0.,-6.5,10.03));
#4172=CARTESIAN_POINT('Origin',(0.,-7.7,10.03));
#4173=CARTESIAN_POINT('Origin',(0.,-9.5,10.03));
#4174=CARTESIAN_POINT('',(-0.7,-6.5,10.03));
#4175=CARTESIAN_POINT('Origin',(0.,-6.5,10.03));
#4176=CARTESIAN_POINT('',(-0.7,-9.5,10.03));
#4177=CARTESIAN_POINT('',(-0.7,-9.5,10.03));
#4178=CARTESIAN_POINT('Origin',(0.,-9.5,10.03));
#4179=CARTESIAN_POINT('Origin',(0.,-6.5,10.03));
#4180=CARTESIAN_POINT('Origin',(0.,-9.5,10.03));
#4181=CARTESIAN_POINT('',(0.,0.,0.));
#4182=CARTESIAN_POINT('Origin',(0.115470053837925,-0.5,-0.2));
#4183=CARTESIAN_POINT('',(0.23094010767585,-0.5,0.));
#4184=CARTESIAN_POINT('',(0.115470053837925,-0.5,-0.2));
#4185=CARTESIAN_POINT('',(0.23094010767585,-0.5,0.));
#4186=CARTESIAN_POINT('',(0.115470053837925,-0.8,-0.2));
#4187=CARTESIAN_POINT('',(0.115470053837925,-0.5,-0.2));
#4188=CARTESIAN_POINT('',(0.23094010767585,-0.8,0.));
#4189=CARTESIAN_POINT('',(0.23094010767585,-0.8,0.));
#4190=CARTESIAN_POINT('',(0.23094010767585,-0.5,0.));
#4191=CARTESIAN_POINT('Origin',(-0.115470053837925,-0.5,-0.2));
#4192=CARTESIAN_POINT('',(-0.115470053837925,-0.5,-0.2));
#4193=CARTESIAN_POINT('',(0.115470053837925,-0.5,-0.2));
#4194=CARTESIAN_POINT('',(-0.115470053837925,-0.8,-0.2));
#4195=CARTESIAN_POINT('',(-0.115470053837925,-0.5,-0.2));
#4196=CARTESIAN_POINT('',(0.115470053837925,-0.8,-0.2));
#4197=CARTESIAN_POINT('Origin',(-0.23094010767585,-0.5,-2.77555756156289E-17));
#4198=CARTESIAN_POINT('',(-0.23094010767585,-0.5,-2.82820063659975E-17));
#4199=CARTESIAN_POINT('',(-0.115470053837925,-0.5,-0.2));
#4200=CARTESIAN_POINT('',(-0.23094010767585,-0.8,-2.77555756156289E-17));
#4201=CARTESIAN_POINT('',(-0.23094010767585,-0.5,-2.82820063659975E-17));
#4202=CARTESIAN_POINT('',(-0.115470053837925,-0.8,-0.2));
#4203=CARTESIAN_POINT('Origin',(-0.115470053837925,-0.5,0.2));
#4204=CARTESIAN_POINT('',(-0.115470053837925,-0.5,0.2));
#4205=CARTESIAN_POINT('',(-0.23094010767585,-0.5,-2.82820063659975E-17));
#4206=CARTESIAN_POINT('',(-0.115470053837925,-0.8,0.2));
#4207=CARTESIAN_POINT('',(-0.115470053837925,-0.5,0.2));
#4208=CARTESIAN_POINT('',(-0.23094010767585,-0.8,-2.82820063659975E-17));
#4209=CARTESIAN_POINT('Origin',(0.115470053837925,-0.5,0.2));
#4210=CARTESIAN_POINT('',(0.115470053837925,-0.5,0.2));
#4211=CARTESIAN_POINT('',(-0.115470053837925,-0.5,0.2));
#4212=CARTESIAN_POINT('',(0.115470053837925,-0.8,0.2));
#4213=CARTESIAN_POINT('',(0.115470053837925,-0.5,0.2));
#4214=CARTESIAN_POINT('',(-0.115470053837925,-0.8,0.2));
#4215=CARTESIAN_POINT('Origin',(0.23094010767585,-0.5,0.));
#4216=CARTESIAN_POINT('',(0.115470053837925,-0.5,0.2));
#4217=CARTESIAN_POINT('',(0.115470053837925,-0.8,0.2));
#4218=CARTESIAN_POINT('Origin',(0.,-0.5,0.));
#4219=CARTESIAN_POINT('Origin',(0.,-0.8,0.));
#4220=CARTESIAN_POINT('Origin',(0.,-1.4,0.));
#4221=CARTESIAN_POINT('',(-0.24505,-1.4,3.00099698131059E-17));
#4222=CARTESIAN_POINT('Origin',(0.,-1.4,0.));
#4223=CARTESIAN_POINT('Origin',(0.375,0.5,0.));
#4224=CARTESIAN_POINT('',(-0.375,0.5,-4.59242549680257E-17));
#4225=CARTESIAN_POINT('Origin',(0.,0.5,0.));
#4226=CARTESIAN_POINT('Origin',(0.,0.475,0.));
#4227=CARTESIAN_POINT('',(-0.425,0.45,-5.20474889637625E-17));
#4228=CARTESIAN_POINT('Origin',(0.,0.45,0.));
#4229=CARTESIAN_POINT('',(-0.4,0.475,-4.89858719658941E-17));
#4230=CARTESIAN_POINT('Origin',(0.,0.24,0.));
#4231=CARTESIAN_POINT('',(-0.425,0.0299999999999998,-5.20474889637625E-17));
#4232=CARTESIAN_POINT('Origin',(0.,0.0299999999999998,0.));
#4233=CARTESIAN_POINT('',(-0.425,0.24,-5.20474889637625E-17));
#4234=CARTESIAN_POINT('Origin',(0.,0.0150000000000001,0.));
#4235=CARTESIAN_POINT('',(-0.395,4.85722573273506E-17,-4.83735485663204E-17));
#4236=CARTESIAN_POINT('Origin',(0.,0.,0.));
#4237=CARTESIAN_POINT('',(-0.41,0.0150000000000001,-5.02105187650415E-17));
#4238=CARTESIAN_POINT('Origin',(0.27,0.,0.));
#4239=CARTESIAN_POINT('',(-0.27,0.,-3.30654635769785E-17));
#4240=CARTESIAN_POINT('Origin',(0.,0.,0.));
#4241=CARTESIAN_POINT('Origin',(0.,-0.02,0.));
#4242=CARTESIAN_POINT('',(-0.24505,-0.0498999999999999,3.00099698131059E-17));
#4243=CARTESIAN_POINT('Origin',(0.,-0.0498999999999999,0.));
#4244=CARTESIAN_POINT('',(-0.26,-0.02,-3.18408167778312E-17));
#4245=CARTESIAN_POINT('Origin',(0.,-0.995,0.));
#4246=CARTESIAN_POINT('',(-0.24505,-0.995,-3.00099698131059E-17));
#4247=CARTESIAN_POINT('',(0.,0.,0.));
#4248=CARTESIAN_POINT('',(0.,0.,0.));
#4249=CARTESIAN_POINT('Origin',(2.49048674522936,-0.6,2.28211064313085));
#4250=CARTESIAN_POINT('',(2.18048674522936,-0.48,2.28211064313085));
#4251=CARTESIAN_POINT('Origin',(2.49048674522936,-0.48,2.28211064313085));
#4252=CARTESIAN_POINT('',(2.18048674522936,0.48,2.28211064313085));
#4253=CARTESIAN_POINT('',(2.18048674522936,-0.6,2.28211064313085));
#4254=CARTESIAN_POINT('Origin',(2.49048674522936,0.48,2.28211064313085));
#4255=CARTESIAN_POINT('Origin',(5.98369790806552,-0.6,2.5));
#4256=CARTESIAN_POINT('',(5.67369790806552,-0.48,2.5));
#4257=CARTESIAN_POINT('Origin',(5.98369790806552,-0.48,2.5));
#4258=CARTESIAN_POINT('',(5.67369790806552,0.48,2.5));
#4259=CARTESIAN_POINT('',(5.67369790806552,-0.6,2.5));
#4260=CARTESIAN_POINT('Origin',(5.98369790806552,0.48,2.5));
#4261=CARTESIAN_POINT('Origin',(5.98369790806552,-0.48,2.5));
#4262=CARTESIAN_POINT('',(5.56225339914413,0.48,2.07293498633112));
#4263=CARTESIAN_POINT('',(5.56225339914413,-0.48,2.07293498633112));
#4264=CARTESIAN_POINT('',(5.56225339914413,-0.48,2.07293498633112));
#4265=CARTESIAN_POINT('',(5.51245011757404,0.48,2.87138325212224));
#4266=CARTESIAN_POINT('Origin',(5.98369790806552,0.48,2.5));
#4267=CARTESIAN_POINT('',(5.51245011757404,-0.48,2.87138325212224));
#4268=CARTESIAN_POINT('',(5.51245011757404,-0.48,2.87138325212224));
#4269=CARTESIAN_POINT('Origin',(5.98369790806552,-0.48,2.5));
#4270=CARTESIAN_POINT('Origin',(6.00859954885057,-0.48,2.10077586710444));
#4271=CARTESIAN_POINT('',(2.96173453572085,-0.48,1.91072739100861));
#4272=CARTESIAN_POINT('',(6.00859954885057,-0.48,2.10077586710444));
#4273=CARTESIAN_POINT('',(2.96173453572085,0.48,1.91072739100861));
#4274=CARTESIAN_POINT('',(2.96173453572085,-0.48,1.91072739100861));
#4275=CARTESIAN_POINT('',(6.00859954885057,0.48,2.10077586710444));
#4276=CARTESIAN_POINT('Origin',(2.49048674522936,-0.48,2.28211064313085));
#4277=CARTESIAN_POINT('',(2.91193125415076,-0.48,2.70917565679974));
#4278=CARTESIAN_POINT('',(2.46558510444432,-0.48,2.68133477602642));
#4279=CARTESIAN_POINT('Origin',(2.49048674522936,-0.48,2.28211064313085));
#4280=CARTESIAN_POINT('Origin',(2.46558510444432,-0.48,2.68133477602642));
#4281=CARTESIAN_POINT('',(2.91193125415076,0.48,2.70917565679974));
#4282=CARTESIAN_POINT('',(2.46558510444432,0.48,2.68133477602642));
#4283=CARTESIAN_POINT('',(2.91193125415076,-0.48,2.70917565679974));
#4284=CARTESIAN_POINT('Origin',(2.49048674522936,-0.48,2.28211064313085));
#4285=CARTESIAN_POINT('Origin',(2.49048674522936,0.48,2.28211064313085));
#4286=CARTESIAN_POINT('Origin',(2.49048674522936,0.48,2.28211064313085));
#4287=CARTESIAN_POINT('',(0.,0.,0.));
#4288=CARTESIAN_POINT('',(0.,0.,0.));
#4289=CARTESIAN_POINT('',(0.,0.,0.));
#4290=CARTESIAN_POINT('Origin',(11.4,0.,2.5));
#4291=CARTESIAN_POINT('',(11.4,-4.163799117101E-17,2.84));
#4292=CARTESIAN_POINT('Origin',(11.4,0.,2.5));
#4293=CARTESIAN_POINT('',(13.,4.163799117101E-17,2.84));
#4294=CARTESIAN_POINT('',(11.4,-4.163799117101E-17,2.84));
#4295=CARTESIAN_POINT('Origin',(13.,0.,2.5));
#4296=CARTESIAN_POINT('Origin',(11.4,0.,2.5));
#4297=CARTESIAN_POINT('Origin',(5.98369790806552,-1.,2.5));
#4298=CARTESIAN_POINT('',(5.67369790806552,-0.9,2.5));
#4299=CARTESIAN_POINT('Origin',(5.98369790806552,-0.9,2.5));
#4300=CARTESIAN_POINT('',(5.67369790806552,-0.5,2.5));
#4301=CARTESIAN_POINT('',(5.67369790806552,-1.,2.5));
#4302=CARTESIAN_POINT('Origin',(5.98369790806552,-0.5,2.5));
#4303=CARTESIAN_POINT('Origin',(5.98369790806552,-1.,2.5));
#4304=CARTESIAN_POINT('',(5.67369790806552,0.5,2.5));
#4305=CARTESIAN_POINT('Origin',(5.98369790806552,0.5,2.5));
#4306=CARTESIAN_POINT('',(5.67369790806552,0.9,2.5));
#4307=CARTESIAN_POINT('',(5.67369790806552,-1.,2.5));
#4308=CARTESIAN_POINT('Origin',(5.98369790806552,0.9,2.5));
#4309=CARTESIAN_POINT('Origin',(6.88369790806552,-0.9,1.7));
#4310=CARTESIAN_POINT('',(6.88369790806552,0.5,1.7));
#4311=CARTESIAN_POINT('',(6.88369790806552,0.5,3.3));
#4312=CARTESIAN_POINT('',(6.88369790806552,0.5,2.1));
#4313=CARTESIAN_POINT('',(6.88369790806552,-0.5,1.7));
#4314=CARTESIAN_POINT('',(6.88369790806552,-0.9,1.7));
#4315=CARTESIAN_POINT('',(6.88369790806552,-0.5,3.3));
#4316=CARTESIAN_POINT('',(6.88369790806552,-0.5,2.1));
#4317=CARTESIAN_POINT('',(6.88369790806552,-0.9,3.3));
#4318=CARTESIAN_POINT('Origin',(6.18369790806552,0.9,2.5));
#4319=CARTESIAN_POINT('',(7.18369790806552,0.9,1.7));
#4320=CARTESIAN_POINT('',(5.18369790806552,0.9,1.7));
#4321=CARTESIAN_POINT('',(5.18369790806552,0.9,1.7));
#4322=CARTESIAN_POINT('',(5.18369790806552,0.9,3.3));
#4323=CARTESIAN_POINT('',(5.18369790806552,0.9,3.3));
#4324=CARTESIAN_POINT('',(7.18369790806552,0.9,3.3));
#4325=CARTESIAN_POINT('',(7.18369790806552,0.9,3.3));
#4326=CARTESIAN_POINT('',(7.18369790806552,0.9,1.7));
#4327=CARTESIAN_POINT('Origin',(7.18369790806552,0.5,1.7));
#4328=CARTESIAN_POINT('',(5.18369790806552,0.5,1.7));
#4329=CARTESIAN_POINT('',(5.18369790806552,0.5,1.7));
#4330=CARTESIAN_POINT('',(5.18369790806552,0.5,1.7));
#4331=CARTESIAN_POINT('',(7.18369790806552,-0.9,1.7));
#4332=CARTESIAN_POINT('',(7.18369790806552,0.5,1.7));
#4333=CARTESIAN_POINT('',(5.18369790806552,-0.9,1.7));
#4334=CARTESIAN_POINT('',(5.18369790806552,-0.9,1.7));
#4335=CARTESIAN_POINT('',(5.18369790806552,-0.5,1.7));
#4336=CARTESIAN_POINT('',(5.18369790806552,-0.9,1.7));
#4337=CARTESIAN_POINT('',(5.18369790806552,-0.5,1.7));
#4338=CARTESIAN_POINT('Origin',(6.18369790806552,-0.9,2.5));
#4339=CARTESIAN_POINT('',(7.18369790806552,-0.9,3.3));
#4340=CARTESIAN_POINT('',(5.18369790806552,-0.9,3.3));
#4341=CARTESIAN_POINT('',(7.18369790806552,-0.9,3.3));
#4342=CARTESIAN_POINT('',(5.18369790806552,-0.9,3.3));
#4343=CARTESIAN_POINT('',(7.18369790806552,-0.9,1.7));
#4344=CARTESIAN_POINT('Origin',(5.18369790806552,0.5,1.7));
#4345=CARTESIAN_POINT('',(5.18369790806552,0.5,3.3));
#4346=CARTESIAN_POINT('',(5.18369790806552,0.5,3.3));
#4347=CARTESIAN_POINT('',(5.18369790806552,0.5,3.3));
#4348=CARTESIAN_POINT('Origin',(7.18369790806552,0.5,3.3));
#4349=CARTESIAN_POINT('',(7.18369790806552,0.5,3.3));
#4350=CARTESIAN_POINT('',(7.18369790806552,-6.12323399573677E-17,3.));
#4351=CARTESIAN_POINT('Origin',(7.18369790806552,0.,2.5));
#4352=CARTESIAN_POINT('Origin',(5.18369790806552,0.5,3.3));
#4353=CARTESIAN_POINT('',(7.18369790806552,0.5,3.3));
#4354=CARTESIAN_POINT('',(5.18369790806552,-0.5,3.3));
#4355=CARTESIAN_POINT('',(7.18369790806552,-0.5,3.3));
#4356=CARTESIAN_POINT('',(5.18369790806552,-0.9,3.3));
#4357=CARTESIAN_POINT('Origin',(6.18369790806552,0.5,2.5));
#4358=CARTESIAN_POINT('Origin',(5.18369790806552,-0.9,1.7));
#4359=CARTESIAN_POINT('',(5.18369790806552,-0.5,3.3));
#4360=CARTESIAN_POINT('Origin',(6.18369790806552,-0.5,2.5));
#4361=CARTESIAN_POINT('Origin',(6.98369791,0.,2.5));
#4362=CARTESIAN_POINT('',(13.,-6.12323399573677E-17,3.));
#4363=CARTESIAN_POINT('Origin',(13.,0.,2.5));
#4364=CARTESIAN_POINT('',(6.98369791,-6.12323399573677E-17,3.));
#4365=CARTESIAN_POINT('Origin',(13.,0.,2.5));
#4366=CARTESIAN_POINT('',(0.,0.,0.));
#4367=CARTESIAN_POINT('Origin',(0.,-1.935,0.));
#4368=CARTESIAN_POINT('',(-0.3933,-3.9267,4.81653586104654E-17));
#4369=CARTESIAN_POINT('Origin',(0.,-3.9267,0.));
#4370=CARTESIAN_POINT('',(-0.3933,0.,-4.81653586104654E-17));
#4371=CARTESIAN_POINT('',(-0.3933,-1.935,-4.81653586104654E-17));
#4372=CARTESIAN_POINT('Origin',(0.,0.,0.));
#4373=CARTESIAN_POINT('Origin',(0.,-3.96,0.));
#4374=CARTESIAN_POINT('',(-0.32,-4.,-3.91886975727153E-17));
#4375=CARTESIAN_POINT('Origin',(0.,-4.,0.));
#4376=CARTESIAN_POINT('',(-0.36,-3.96,-4.40872847693047E-17));
#4377=CARTESIAN_POINT('Origin',(0.,-4.,0.));
#4378=CARTESIAN_POINT('Origin',(0.,0.462722715486149,0.));
#4379=CARTESIAN_POINT('',(-0.6175,0.53,-7.5621939847349E-17));
#4380=CARTESIAN_POINT('Origin',(0.,0.53,0.));
#4381=CARTESIAN_POINT('',(-0.750555349946514,0.453180457891261,-9.19165206894919E-17));
#4382=CARTESIAN_POINT('',(-0.734027674973257,0.462722715486149,-8.98924642641573E-17));
#4383=CARTESIAN_POINT('',(-0.375277674973257,0.453180457891261,0.65));
#4384=CARTESIAN_POINT('Ctrl Pts',(-0.375277674973257,0.45318045789126,0.65));
#4385=CARTESIAN_POINT('Ctrl Pts',(-0.562916512459968,0.561513791224244,
0.324999999999856));
#4386=CARTESIAN_POINT('Ctrl Pts',(-0.750555349946514,0.45318045789126,-9.19165206894919E-17));
#4387=CARTESIAN_POINT('',(0.375277674973257,0.453180457891261,0.65));
#4388=CARTESIAN_POINT('Ctrl Pts',(0.375277674973257,0.453180457891261,0.65));
#4389=CARTESIAN_POINT('Ctrl Pts',(-1.66922031752392E-13,0.561513791224244,
0.65));
#4390=CARTESIAN_POINT('Ctrl Pts',(-0.375277674973257,0.45318045789126,0.65));
#4391=CARTESIAN_POINT('',(0.750555349946514,0.453180457891261,0.));
#4392=CARTESIAN_POINT('Ctrl Pts',(0.750555349946514,0.453180457891261,0.));
#4393=CARTESIAN_POINT('Ctrl Pts',(0.562916512459802,0.561513791224244,0.325000000000144));
#4394=CARTESIAN_POINT('Ctrl Pts',(0.375277674973257,0.45318045789126,0.65));
#4395=CARTESIAN_POINT('',(0.375277674973257,0.453180457891261,-0.65));
#4396=CARTESIAN_POINT('Ctrl Pts',(0.375277674973257,0.45318045789126,-0.65));
#4397=CARTESIAN_POINT('Ctrl Pts',(0.562916512459968,0.561513791224244,-0.324999999999855));
#4398=CARTESIAN_POINT('Ctrl Pts',(0.750555349946514,0.453180457891261,0.));
#4399=CARTESIAN_POINT('',(-0.375277674973257,0.45318045789126,-0.65));
#4400=CARTESIAN_POINT('Ctrl Pts',(-0.375277674973257,0.453180457891261,
-0.65));
#4401=CARTESIAN_POINT('Ctrl Pts',(1.66866520601161E-13,0.561513791224244,
-0.65));
#4402=CARTESIAN_POINT('Ctrl Pts',(0.375277674973257,0.45318045789126,-0.65));
#4403=CARTESIAN_POINT('Ctrl Pts',(-0.750555349946514,0.453180457891261,
-9.19165206894919E-17));
#4404=CARTESIAN_POINT('Ctrl Pts',(-0.562916512459802,0.561513791224244,
-0.325000000000144));
#4405=CARTESIAN_POINT('Ctrl Pts',(-0.375277674973257,0.45318045789126,-0.65));
#4406=CARTESIAN_POINT('Origin',(0.375277674973257,0.,-0.65));
#4407=CARTESIAN_POINT('',(0.375277674973257,0.,-0.65));
#4408=CARTESIAN_POINT('',(0.375277674973257,0.,-0.65));
#4409=CARTESIAN_POINT('',(-0.375277674973257,0.,-0.65));
#4410=CARTESIAN_POINT('',(0.375277674973257,0.,-0.65));
#4411=CARTESIAN_POINT('',(-0.375277674973257,0.,-0.65));
#4412=CARTESIAN_POINT('Origin',(0.750555349946514,0.,0.));
#4413=CARTESIAN_POINT('',(0.750555349946514,0.,0.));
#4414=CARTESIAN_POINT('',(0.750555349946514,0.,0.));
#4415=CARTESIAN_POINT('',(0.750555349946514,0.,0.));
#4416=CARTESIAN_POINT('Origin',(0.375277674973257,0.,0.65));
#4417=CARTESIAN_POINT('',(0.375277674973257,0.,0.65));
#4418=CARTESIAN_POINT('',(0.375277674973257,0.,0.65));
#4419=CARTESIAN_POINT('',(0.375277674973257,0.,0.65));
#4420=CARTESIAN_POINT('Origin',(-0.375277674973257,0.,0.65));
#4421=CARTESIAN_POINT('',(-0.375277674973257,0.,0.65));
#4422=CARTESIAN_POINT('',(-0.375277674973257,0.,0.65));
#4423=CARTESIAN_POINT('',(-0.375277674973257,0.,0.65));
#4424=CARTESIAN_POINT('Origin',(-0.750555349946514,0.,-9.19165206894919E-17));
#4425=CARTESIAN_POINT('',(-0.750555349946514,0.,-9.19165206894919E-17));
#4426=CARTESIAN_POINT('',(-0.750555349946514,0.,-9.19165206894919E-17));
#4427=CARTESIAN_POINT('',(-0.750555349946514,0.,-9.19165206894919E-17));
#4428=CARTESIAN_POINT('Origin',(-0.375277674973257,0.,-0.65));
#4429=CARTESIAN_POINT('',(-0.375277674973257,0.,-0.65));
#4430=CARTESIAN_POINT('Origin',(0.,0.53,-1.11022302462516E-16));
#4431=CARTESIAN_POINT('Origin',(0.,0.,-1.11022302462516E-16));
#4432=CARTESIAN_POINT('',(0.,0.,0.));
#4433=CARTESIAN_POINT('Origin',(0.,0.067277284513851,0.));
#4434=CARTESIAN_POINT('',(-0.375277674973257,0.0768195421087395,0.65));
#4435=CARTESIAN_POINT('',(0.375277674973257,0.0768195421087395,0.65));
#4436=CARTESIAN_POINT('Ctrl Pts',(-0.375277674973257,0.0768195421087395,
0.65));
#4437=CARTESIAN_POINT('Ctrl Pts',(1.66533453693773E-13,-0.0315137912242439,
0.65));
#4438=CARTESIAN_POINT('Ctrl Pts',(0.375277674973257,0.0768195421087394,
0.65));
#4439=CARTESIAN_POINT('',(-0.750555349946514,0.0768195421087394,-9.19165206894919E-17));
#4440=CARTESIAN_POINT('Ctrl Pts',(-0.750555349946514,0.0768195421087394,
-9.19165206894919E-17));
#4441=CARTESIAN_POINT('Ctrl Pts',(-0.562916512459802,-0.0315137912242434,
0.325000000000144));
#4442=CARTESIAN_POINT('Ctrl Pts',(-0.375277674973257,0.0768195421087395,
0.65));
#4443=CARTESIAN_POINT('',(-0.6175,-2.77555756156289E-17,-7.5621939847349E-17));
#4444=CARTESIAN_POINT('',(-0.734027674973257,0.067277284513851,-8.98924642641573E-17));
#4445=CARTESIAN_POINT('Origin',(0.,0.,0.));
#4446=CARTESIAN_POINT('',(-0.375277674973257,0.0768195421087395,-0.65));
#4447=CARTESIAN_POINT('Ctrl Pts',(-0.375277674973257,0.0768195421087395,
-0.65));
#4448=CARTESIAN_POINT('Ctrl Pts',(-0.562916512459968,-0.0315137912242437,
-0.324999999999856));
#4449=CARTESIAN_POINT('Ctrl Pts',(-0.750555349946514,0.0768195421087395,
-9.19165206894919E-17));
#4450=CARTESIAN_POINT('',(0.375277674973257,0.0768195421087395,-0.65));
#4451=CARTESIAN_POINT('Ctrl Pts',(0.375277674973257,0.0768195421087395,
-0.65));
#4452=CARTESIAN_POINT('Ctrl Pts',(-1.66144875635155E-13,-0.0315137912242437,
-0.65));
#4453=CARTESIAN_POINT('Ctrl Pts',(-0.375277674973257,0.0768195421087395,
-0.65));
#4454=CARTESIAN_POINT('',(0.750555349946514,0.0768195421087394,0.));
#4455=CARTESIAN_POINT('Ctrl Pts',(0.750555349946514,0.0768195421087394,
0.));
#4456=CARTESIAN_POINT('Ctrl Pts',(0.562916512459802,-0.0315137912242436,
-0.325000000000144));
#4457=CARTESIAN_POINT('Ctrl Pts',(0.375277674973257,0.0768195421087395,
-0.65));
#4458=CARTESIAN_POINT('Ctrl Pts',(0.375277674973257,0.0768195421087394,
0.65));
#4459=CARTESIAN_POINT('Ctrl Pts',(0.562916512459968,-0.0315137912242439,
0.324999999999856));
#4460=CARTESIAN_POINT('Ctrl Pts',(0.750555349946514,0.0768195421087394,
0.));
#4461=CARTESIAN_POINT('Origin',(0.,0.612722715486149,0.));
#4462=CARTESIAN_POINT('',(-0.6175,0.68,-7.5621939847349E-17));
#4463=CARTESIAN_POINT('Origin',(0.,0.68,0.));
#4464=CARTESIAN_POINT('',(-0.750555349946514,0.603180457891261,-9.19165206894919E-17));
#4465=CARTESIAN_POINT('',(-0.734027674973257,0.612722715486149,-8.98924642641573E-17));
#4466=CARTESIAN_POINT('',(-0.375277674973257,0.603180457891261,0.65));
#4467=CARTESIAN_POINT('Ctrl Pts',(-0.375277674973257,0.603180457891261,
0.65));
#4468=CARTESIAN_POINT('Ctrl Pts',(-0.562916512459968,0.711513791224243,
0.324999999999856));
#4469=CARTESIAN_POINT('Ctrl Pts',(-0.750555349946514,0.603180457891261,
-9.19165206894919E-17));
#4470=CARTESIAN_POINT('',(0.375277674973257,0.603180457891261,0.65));
#4471=CARTESIAN_POINT('Ctrl Pts',(0.375277674973257,0.603180457891261,0.65));
#4472=CARTESIAN_POINT('Ctrl Pts',(-1.66755498298699E-13,0.711513791224244,
0.65));
#4473=CARTESIAN_POINT('Ctrl Pts',(-0.375277674973257,0.603180457891261,
0.65));
#4474=CARTESIAN_POINT('',(0.750555349946514,0.603180457891261,0.));
#4475=CARTESIAN_POINT('Ctrl Pts',(0.750555349946514,0.603180457891261,0.));
#4476=CARTESIAN_POINT('Ctrl Pts',(0.562916512459802,0.711513791224244,0.325000000000144));
#4477=CARTESIAN_POINT('Ctrl Pts',(0.375277674973257,0.603180457891261,0.65));
#4478=CARTESIAN_POINT('',(0.375277674973257,0.603180457891261,-0.65));
#4479=CARTESIAN_POINT('Ctrl Pts',(0.375277674973257,0.603180457891261,-0.65));
#4480=CARTESIAN_POINT('Ctrl Pts',(0.562916512459969,0.711513791224244,-0.324999999999856));
#4481=CARTESIAN_POINT('Ctrl Pts',(0.750555349946514,0.603180457891261,0.));
#4482=CARTESIAN_POINT('',(-0.375277674973257,0.603180457891261,-0.65));
#4483=CARTESIAN_POINT('Ctrl Pts',(-0.375277674973257,0.603180457891261,
-0.65));
#4484=CARTESIAN_POINT('Ctrl Pts',(1.66422431391311E-13,0.711513791224244,
-0.65));
#4485=CARTESIAN_POINT('Ctrl Pts',(0.375277674973257,0.603180457891261,-0.65));
#4486=CARTESIAN_POINT('Ctrl Pts',(-0.750555349946514,0.603180457891261,
-9.19165206894919E-17));
#4487=CARTESIAN_POINT('Ctrl Pts',(-0.562916512459802,0.711513791224244,
-0.325000000000144));
#4488=CARTESIAN_POINT('Ctrl Pts',(-0.375277674973257,0.603180457891261,
-0.65));
#4489=CARTESIAN_POINT('Origin',(0.375277674973257,0.,-0.65));
#4490=CARTESIAN_POINT('',(-0.375277674973257,0.,-0.65));
#4491=CARTESIAN_POINT('',(0.375277674973257,0.,-0.65));
#4492=CARTESIAN_POINT('Origin',(-0.375277674973257,0.,-0.65));
#4493=CARTESIAN_POINT('',(-0.750555349946514,0.,-9.19165206894919E-17));
#4494=CARTESIAN_POINT('Origin',(-0.750555349946514,0.,-9.19165206894919E-17));
#4495=CARTESIAN_POINT('',(-0.375277674973257,0.,0.65));
#4496=CARTESIAN_POINT('Origin',(0.,0.,0.));
#4497=CARTESIAN_POINT('',(-0.338975,0.68,4.15124648740974E-17));
#4498=CARTESIAN_POINT('Origin',(0.,0.68,0.));
#4499=CARTESIAN_POINT('',(-0.338975,0.,4.15124648740974E-17));
#4500=CARTESIAN_POINT('',(-0.338975,0.,4.15124648740974E-17));
#4501=CARTESIAN_POINT('Origin',(0.,0.,0.));
#4502=CARTESIAN_POINT('Origin',(-0.375277674973257,0.,0.65));
#4503=CARTESIAN_POINT('',(0.375277674973257,0.,0.65));
#4504=CARTESIAN_POINT('Origin',(0.750555349946514,0.,0.));
#4505=CARTESIAN_POINT('',(0.750555349946514,0.,0.));
#4506=CARTESIAN_POINT('Origin',(0.375277674973257,0.,0.65));
#4507=CARTESIAN_POINT('Origin',(0.,0.68,-1.11022302462516E-16));
#4508=CARTESIAN_POINT('Origin',(0.,0.,-1.11022302462516E-16));
#4509=CARTESIAN_POINT('',(0.,0.,0.));
#4510=CARTESIAN_POINT('Origin',(0.,0.,3.));
#4511=CARTESIAN_POINT('',(-1.,-1.22464679914735E-16,3.4));
#4512=CARTESIAN_POINT('Origin',(0.,0.,3.4));
#4513=CARTESIAN_POINT('',(-1.,-1.22464679914735E-16,3.));
#4514=CARTESIAN_POINT('',(-1.,-1.22464679914735E-16,3.));
#4515=CARTESIAN_POINT('Origin',(0.,0.,3.));
#4516=CARTESIAN_POINT('Origin',(0.,0.,3.4));
#4517=CARTESIAN_POINT('Origin',(0.,0.,3.));
#4518=CARTESIAN_POINT('',(0.,0.,0.));
#4519=CARTESIAN_POINT('Origin',(0.,-2.7,0.));
#4520=CARTESIAN_POINT('',(-0.289136645896019,-2.7,0.08));
#4521=CARTESIAN_POINT('',(-0.3,-2.78,-2.27065106771523E-17));
#4522=CARTESIAN_POINT('Ctrl Pts',(-0.289136645896019,-2.7,0.08));
#4523=CARTESIAN_POINT('Ctrl Pts',(-0.289136645896019,-2.71009877520201,
0.08));
#4524=CARTESIAN_POINT('Ctrl Pts',(-0.289720927595908,-2.72083518625944,
0.0779717130936404));
#4525=CARTESIAN_POINT('Ctrl Pts',(-0.291799203044223,-2.74052980652726,
0.0697927537456149));
#4526=CARTESIAN_POINT('Ctrl Pts',(-0.293259762986909,-2.74949254880105,
0.0636445361887959));
#4527=CARTESIAN_POINT('Ctrl Pts',(-0.295976783522942,-2.76364324458222,
0.0494938404076284));
#4528=CARTESIAN_POINT('Ctrl Pts',(-0.297414335384467,-2.76979246713824,
0.0405305642602551));
#4529=CARTESIAN_POINT('Ctrl Pts',(-0.299439403644655,-2.77797216257078,
0.0208340363410407));
#4530=CARTESIAN_POINT('Ctrl Pts',(-0.3,-2.78,0.0100969318362556));
#4531=CARTESIAN_POINT('Ctrl Pts',(-0.3,-2.78,5.20417042793042E-18));
#4532=CARTESIAN_POINT('',(0.289136645896019,-2.7,0.08));
#4533=CARTESIAN_POINT('',(0.,-2.7,0.08));
#4534=CARTESIAN_POINT('Ctrl Pts',(0.289136645896019,-2.7,0.08));
#4535=CARTESIAN_POINT('Ctrl Pts',(0.289136645896019,-2.68990122479799,0.08));
#4536=CARTESIAN_POINT('Ctrl Pts',(0.289720927595908,-2.67916481374056,0.0779717130936404));
#4537=CARTESIAN_POINT('Ctrl Pts',(0.291799203044223,-2.65947019347274,0.0697927537456147));
#4538=CARTESIAN_POINT('Ctrl Pts',(0.293259762986909,-2.65050745119895,0.0636445361887959));
#4539=CARTESIAN_POINT('Ctrl Pts',(0.295976783522942,-2.63635675541778,0.0494938404076283));
#4540=CARTESIAN_POINT('Ctrl Pts',(0.297414335384467,-2.63020753286176,0.0405305642602551));
#4541=CARTESIAN_POINT('Ctrl Pts',(0.299439403644655,-2.62202783742922,0.0208340363410406));
#4542=CARTESIAN_POINT('Ctrl Pts',(0.3,-2.62,0.0100969318362555));
#4543=CARTESIAN_POINT('Ctrl Pts',(0.3,-2.62,-0.0100969318362556));
#4544=CARTESIAN_POINT('Ctrl Pts',(0.299439403644655,-2.62202783742922,-0.0208340363410406));
#4545=CARTESIAN_POINT('Ctrl Pts',(0.297414335384467,-2.63020753286176,-0.0405305642602551));
#4546=CARTESIAN_POINT('Ctrl Pts',(0.295976783522942,-2.63635675541778,-0.0494938404076283));
#4547=CARTESIAN_POINT('Ctrl Pts',(0.293259762986909,-2.65050745119895,-0.0636445361887959));
#4548=CARTESIAN_POINT('Ctrl Pts',(0.291799203044223,-2.65947019347274,-0.0697927537456147));
#4549=CARTESIAN_POINT('Ctrl Pts',(0.289720927595908,-2.67916481374056,-0.0779717130936403));
#4550=CARTESIAN_POINT('Ctrl Pts',(0.289136645896019,-2.68990122479799,-0.08));
#4551=CARTESIAN_POINT('Ctrl Pts',(0.289136645896019,-2.71009877520201,-0.08));
#4552=CARTESIAN_POINT('Ctrl Pts',(0.289720927595908,-2.72083518625944,-0.0779717130936404));
#4553=CARTESIAN_POINT('Ctrl Pts',(0.291799203044223,-2.74052980652726,-0.0697927537456147));
#4554=CARTESIAN_POINT('Ctrl Pts',(0.293259762986909,-2.74949254880105,-0.0636445361887959));
#4555=CARTESIAN_POINT('Ctrl Pts',(0.295976783522942,-2.76364324458222,-0.0494938404076283));
#4556=CARTESIAN_POINT('Ctrl Pts',(0.297414335384467,-2.76979246713824,-0.0405305642602551));
#4557=CARTESIAN_POINT('Ctrl Pts',(0.299439403644655,-2.77797216257078,-0.0208340363410406));
#4558=CARTESIAN_POINT('Ctrl Pts',(0.3,-2.78,-0.0100969318362555));
#4559=CARTESIAN_POINT('Ctrl Pts',(0.3,-2.78,0.0100969318362556));
#4560=CARTESIAN_POINT('Ctrl Pts',(0.299439403644655,-2.77797216257078,0.0208340363410407));
#4561=CARTESIAN_POINT('Ctrl Pts',(0.297414335384467,-2.76979246713824,0.0405305642602551));
#4562=CARTESIAN_POINT('Ctrl Pts',(0.295976783522942,-2.76364324458222,0.0494938404076284));
#4563=CARTESIAN_POINT('Ctrl Pts',(0.293259762986909,-2.74949254880105,0.0636445361887959));
#4564=CARTESIAN_POINT('Ctrl Pts',(0.291799203044223,-2.74052980652726,0.0697927537456149));
#4565=CARTESIAN_POINT('Ctrl Pts',(0.289720927595908,-2.72083518625944,0.0779717130936404));
#4566=CARTESIAN_POINT('Ctrl Pts',(0.289136645896019,-2.71009877520201,0.08));
#4567=CARTESIAN_POINT('Ctrl Pts',(0.289136645896019,-2.7,0.08));
#4568=CARTESIAN_POINT('',(-0.3,-2.62,-3.65842984849668E-17));
#4569=CARTESIAN_POINT('Ctrl Pts',(-0.3,-2.62,-3.81639164714898E-17));
#4570=CARTESIAN_POINT('Ctrl Pts',(-0.3,-2.62,0.0100969318362555));
#4571=CARTESIAN_POINT('Ctrl Pts',(-0.299439403644655,-2.62202783742922,
0.0208340363410406));
#4572=CARTESIAN_POINT('Ctrl Pts',(-0.297414335384467,-2.63020753286176,
0.040530564260255));
#4573=CARTESIAN_POINT('Ctrl Pts',(-0.295976783522942,-2.63635675541778,
0.0494938404076283));
#4574=CARTESIAN_POINT('Ctrl Pts',(-0.293259762986909,-2.65050745119895,
0.0636445361887959));
#4575=CARTESIAN_POINT('Ctrl Pts',(-0.291799203044223,-2.65947019347274,
0.0697927537456147));
#4576=CARTESIAN_POINT('Ctrl Pts',(-0.289720927595908,-2.67916481374056,
0.0779717130936404));
#4577=CARTESIAN_POINT('Ctrl Pts',(-0.289136645896019,-2.68990122479799,
0.08));
#4578=CARTESIAN_POINT('Ctrl Pts',(-0.289136645896019,-2.7,0.08));
#4579=CARTESIAN_POINT('Ctrl Pts',(-0.3,-2.78,-6.93889390390723E-18));
#4580=CARTESIAN_POINT('Ctrl Pts',(-0.3,-2.78,-0.0100969318362556));
#4581=CARTESIAN_POINT('Ctrl Pts',(-0.299439403644655,-2.77797216257078,
-0.0208340363410406));
#4582=CARTESIAN_POINT('Ctrl Pts',(-0.297414335384467,-2.76979246713824,
-0.0405305642602551));
#4583=CARTESIAN_POINT('Ctrl Pts',(-0.295976783522942,-2.76364324458222,
-0.0494938404076283));
#4584=CARTESIAN_POINT('Ctrl Pts',(-0.293259762986909,-2.74949254880105,
-0.0636445361887959));
#4585=CARTESIAN_POINT('Ctrl Pts',(-0.291799203044223,-2.74052980652726,
-0.0697927537456147));
#4586=CARTESIAN_POINT('Ctrl Pts',(-0.289720927595908,-2.72083518625944,
-0.0779717130936403));
#4587=CARTESIAN_POINT('Ctrl Pts',(-0.289136645896019,-2.71009877520201,
-0.08));
#4588=CARTESIAN_POINT('Ctrl Pts',(-0.289136645896019,-2.68990122479799,
-0.08));
#4589=CARTESIAN_POINT('Ctrl Pts',(-0.289720927595908,-2.67916481374056,
-0.0779717130936403));
#4590=CARTESIAN_POINT('Ctrl Pts',(-0.291799203044223,-2.65947019347274,
-0.0697927537456147));
#4591=CARTESIAN_POINT('Ctrl Pts',(-0.293259762986909,-2.65050745119895,
-0.0636445361887959));
#4592=CARTESIAN_POINT('Ctrl Pts',(-0.295976783522942,-2.63635675541778,
-0.0494938404076283));
#4593=CARTESIAN_POINT('Ctrl Pts',(-0.297414335384467,-2.63020753286176,
-0.0405305642602551));
#4594=CARTESIAN_POINT('Ctrl Pts',(-0.299439403644655,-2.62202783742922,
-0.0208340363410406));
#4595=CARTESIAN_POINT('Ctrl Pts',(-0.3,-2.62,-0.0100969318362556));
#4596=CARTESIAN_POINT('Ctrl Pts',(-0.3,-2.62,-1.56125112837913E-17));
#4597=CARTESIAN_POINT('Origin',(0.45,0.2,0.));
#4598=CARTESIAN_POINT('',(-0.45,0.2,-5.51091059616309E-17));
#4599=CARTESIAN_POINT('Origin',(0.,0.2,0.));
#4600=CARTESIAN_POINT('Origin',(0.,0.175,0.));
#4601=CARTESIAN_POINT('',(-0.5,0.15,-6.12323399573676E-17));
#4602=CARTESIAN_POINT('Origin',(0.,0.15,0.));
#4603=CARTESIAN_POINT('',(-0.475,0.175,-5.81707229594993E-17));
#4604=CARTESIAN_POINT('Origin',(0.,0.0750000000000002,0.));
#4605=CARTESIAN_POINT('',(-0.5,0.,-6.12323399573677E-17));
#4606=CARTESIAN_POINT('Origin',(0.,0.,0.));
#4607=CARTESIAN_POINT('',(-0.5,0.0750000000000002,-6.12323399573677E-17));
#4608=CARTESIAN_POINT('Origin',(0.3,0.,0.));
#4609=CARTESIAN_POINT('',(-0.3,0.,-3.67394039744206E-17));
#4610=CARTESIAN_POINT('Origin',(0.,0.,0.));
#4611=CARTESIAN_POINT('Origin',(0.,-1.455,0.));
#4612=CARTESIAN_POINT('',(-0.3,-2.91,-3.67394039744206E-17));
#4613=CARTESIAN_POINT('Origin',(0.,-2.91,0.));
#4614=CARTESIAN_POINT('',(-0.3,-1.455,-3.67394039744206E-17));
#4615=CARTESIAN_POINT('',(-0.3,-1.455,-3.67394039744206E-17));
#4616=CARTESIAN_POINT('Origin',(0.,-2.955,0.));
#4617=CARTESIAN_POINT('',(-0.21,-3.,-2.57175827820944E-17));
#4618=CARTESIAN_POINT('Origin',(0.,-3.,0.));
#4619=CARTESIAN_POINT('',(-0.255,-2.955,-3.12284933782575E-17));
#4620=CARTESIAN_POINT('Origin',(0.,-3.,0.));
#4621=CARTESIAN_POINT('',(0.,0.,0.));
#4622=CARTESIAN_POINT('Origin',(0.,0.,0.));
#4623=CARTESIAN_POINT('',(-0.32,0.16,3.91886975727153E-17));
#4624=CARTESIAN_POINT('Origin',(0.,0.16,0.));
#4625=CARTESIAN_POINT('',(-0.32,0.,3.91886975727153E-17));
#4626=CARTESIAN_POINT('',(-0.32,0.,3.91886975727153E-17));
#4627=CARTESIAN_POINT('Origin',(0.,0.,0.));
#4628=CARTESIAN_POINT('Origin',(0.,0.,0.));
#4629=CARTESIAN_POINT('',(-0.6,0.16,7.34788079488412E-17));
#4630=CARTESIAN_POINT('Origin',(0.,0.16,0.));
#4631=CARTESIAN_POINT('',(-0.6,0.,7.34788079488412E-17));
#4632=CARTESIAN_POINT('',(-0.6,0.,7.34788079488412E-17));
#4633=CARTESIAN_POINT('Origin',(0.,0.,0.));
#4634=CARTESIAN_POINT('Origin',(0.,0.16,0.));
#4635=CARTESIAN_POINT('Origin',(0.,0.,0.));
#4636=CARTESIAN_POINT('',(0.,0.,0.));
#4637=CARTESIAN_POINT('Origin',(0.,-1.54,2.5));
#4638=CARTESIAN_POINT('',(-0.31,-1.06,2.5));
#4639=CARTESIAN_POINT('Origin',(0.,-1.06,2.5));
#4640=CARTESIAN_POINT('',(-0.31,-1.54,2.5));
#4641=CARTESIAN_POINT('',(-0.31,-1.54,2.5));
#4642=CARTESIAN_POINT('Origin',(0.,-1.54,2.5));
#4643=CARTESIAN_POINT('Origin',(0.,-1.54,2.5));
#4644=CARTESIAN_POINT('',(-0.5,-1.06,2.5));
#4645=CARTESIAN_POINT('Origin',(0.,-1.06,2.5));
#4646=CARTESIAN_POINT('',(-0.5,-1.54,2.5));
#4647=CARTESIAN_POINT('',(-0.5,-1.54,2.5));
#4648=CARTESIAN_POINT('Origin',(0.,-1.54,2.5));
#4649=CARTESIAN_POINT('Origin',(0.,-1.06,2.5));
#4650=CARTESIAN_POINT('Origin',(0.,-1.54,2.5));
#4651=CARTESIAN_POINT('',(0.,0.,0.));
#4652=CARTESIAN_POINT('Origin',(0.,0.12,0.));
#4653=CARTESIAN_POINT('',(-9.79717439317883E-18,0.12,-0.04));
#4654=CARTESIAN_POINT('Origin',(0.,0.12,-0.12));
#4655=CARTESIAN_POINT('Origin',(9.79717439317883E-18,0.12,0.));
#4656=CARTESIAN_POINT('',(0.08,-4.89858719658941E-18,7.34788079488412E-18));
#4657=CARTESIAN_POINT('',(-0.08,-4.89858719658941E-18,7.34788079488412E-18));
#4658=CARTESIAN_POINT('Ctrl Pts',(0.08,-4.89858719658941E-18,7.34788079488412E-18));
#4659=CARTESIAN_POINT('Ctrl Pts',(0.08,-0.00012864962353541,0.000128649623535413));
#4660=CARTESIAN_POINT('Ctrl Pts',(0.0799996896739287,-0.00025719571182076,
0.000257402596003253));
#4661=CARTESIAN_POINT('Ctrl Pts',(0.0799669711262291,-0.00701193164572964,
0.00703384588894362));
#4662=CARTESIAN_POINT('Ctrl Pts',(0.0791054994909294,-0.0133457972655825,
0.0139383126556792));
#4663=CARTESIAN_POINT('Ctrl Pts',(0.0749700088488058,-0.0265076530862524,
0.0292212026164895));
#4664=CARTESIAN_POINT('Ctrl Pts',(0.0712702072865517,-0.0331317062461458,
0.0375603420117568));
#4665=CARTESIAN_POINT('Ctrl Pts',(0.0612858949407667,-0.0440683985740427,
0.0520545604187517));
#4666=CARTESIAN_POINT('Ctrl Pts',(0.0555090276731744,-0.0485199197794574,
0.0582717815295611));
#4667=CARTESIAN_POINT('Ctrl Pts',(0.0412398082144208,-0.0561090538733877,
0.0691638397919718));
#4668=CARTESIAN_POINT('Ctrl Pts',(0.0327878980890048,-0.059089642483296,
0.0736229049587921));
#4669=CARTESIAN_POINT('Ctrl Pts',(0.0159233027310102,-0.0625179833270725,
0.0787936360751706));
#4670=CARTESIAN_POINT('Ctrl Pts',(0.00801661414593076,-0.0633030277982336,
0.08));
#4671=CARTESIAN_POINT('Ctrl Pts',(-0.00801661414593074,-0.0633030277982336,
0.08));
#4672=CARTESIAN_POINT('Ctrl Pts',(-0.0159233027310102,-0.0625179833270726,
0.0787936360751706));
#4673=CARTESIAN_POINT('Ctrl Pts',(-0.0327878980890049,-0.059089642483296,
0.0736229049587921));
#4674=CARTESIAN_POINT('Ctrl Pts',(-0.0412398082144209,-0.0561090538733877,
0.0691638397919717));
#4675=CARTESIAN_POINT('Ctrl Pts',(-0.0555090276731744,-0.0485199197794574,
0.0582717815295611));
#4676=CARTESIAN_POINT('Ctrl Pts',(-0.0612858949407667,-0.0440683985740427,
0.0520545604187517));
#4677=CARTESIAN_POINT('Ctrl Pts',(-0.0712702072865517,-0.0331317062461458,
0.0375603420117568));
#4678=CARTESIAN_POINT('Ctrl Pts',(-0.0749700088488058,-0.0265076530862524,
0.0292212026164895));
#4679=CARTESIAN_POINT('Ctrl Pts',(-0.0791054994909264,-0.0133457972655921,
0.0139383126556903));
#4680=CARTESIAN_POINT('Ctrl Pts',(-0.0799669711262287,-0.00701193164579759,
0.0070338458890125));
#4681=CARTESIAN_POINT('Ctrl Pts',(-0.0799996896739287,-0.000257195711817665,
0.000257402596000083));
#4682=CARTESIAN_POINT('Ctrl Pts',(-0.08,-0.000128649623538514,0.000128649623538516));
#4683=CARTESIAN_POINT('Ctrl Pts',(-0.08,-4.89858719658941E-18,7.34788079488412E-18));
#4684=CARTESIAN_POINT('Ctrl Pts',(-0.08,-4.89858719658941E-18,7.34788079488412E-18));
#4685=CARTESIAN_POINT('Ctrl Pts',(-0.08,-0.000128649623536042,-0.00012864962353603));
#4686=CARTESIAN_POINT('Ctrl Pts',(-0.0799996896739287,-0.000257195711820127,
-0.000257402596002604));
#4687=CARTESIAN_POINT('Ctrl Pts',(-0.0799669711262289,-0.0070119316457589,
-0.00703384588897312));
#4688=CARTESIAN_POINT('Ctrl Pts',(-0.0791054994909281,-0.0133457972655867,
-0.0139383126556841));
#4689=CARTESIAN_POINT('Ctrl Pts',(-0.0749700088488058,-0.0265076530862525,
-0.0292212026164896));
#4690=CARTESIAN_POINT('Ctrl Pts',(-0.0712702072865516,-0.0331317062461459,
-0.0375603420117568));
#4691=CARTESIAN_POINT('Ctrl Pts',(-0.0612858949407667,-0.0440683985740427,
-0.0520545604187517));
#4692=CARTESIAN_POINT('Ctrl Pts',(-0.0555090276731744,-0.0485199197794574,
-0.0582717815295611));
#4693=CARTESIAN_POINT('Ctrl Pts',(-0.0412398082144209,-0.0561090538733877,
-0.0691638397919717));
#4694=CARTESIAN_POINT('Ctrl Pts',(-0.0327878980890049,-0.059089642483296,
-0.0736229049587921));
#4695=CARTESIAN_POINT('Ctrl Pts',(-0.0159233027310101,-0.0625179833270725,
-0.0787936360751706));
#4696=CARTESIAN_POINT('Ctrl Pts',(-0.00801661414593069,-0.0633030277982336,
-0.08));
#4697=CARTESIAN_POINT('Ctrl Pts',(0.0080166141459307,-0.0633030277982336,
-0.08));
#4698=CARTESIAN_POINT('Ctrl Pts',(0.0159233027310101,-0.0625179833270725,
-0.0787936360751706));
#4699=CARTESIAN_POINT('Ctrl Pts',(0.0327878980890049,-0.0590896424832959,
-0.0736229049587921));
#4700=CARTESIAN_POINT('Ctrl Pts',(0.0412398082144209,-0.0561090538733877,
-0.0691638397919717));
#4701=CARTESIAN_POINT('Ctrl Pts',(0.0555090276731744,-0.0485199197794574,
-0.0582717815295611));
#4702=CARTESIAN_POINT('Ctrl Pts',(0.0612858949407666,-0.0440683985740428,
-0.0520545604187518));
#4703=CARTESIAN_POINT('Ctrl Pts',(0.0712702072865517,-0.0331317062461458,
-0.0375603420117568));
#4704=CARTESIAN_POINT('Ctrl Pts',(0.0749700088488058,-0.0265076530862524,
-0.0292212026164895));
#4705=CARTESIAN_POINT('Ctrl Pts',(0.079105499490928,-0.013345797265587,
-0.0139383126556845));
#4706=CARTESIAN_POINT('Ctrl Pts',(0.0799669711262289,-0.00701193164576148,
-0.00703384588897579));
#4707=CARTESIAN_POINT('Ctrl Pts',(0.0799996896739287,-0.000257195711819584,
-0.000257402596002039));
#4708=CARTESIAN_POINT('Ctrl Pts',(0.08,-0.000128649623536605,-0.000128649623536593));
#4709=CARTESIAN_POINT('Ctrl Pts',(0.08,-4.89858719658941E-18,7.34788079488412E-18));
#4710=CARTESIAN_POINT('Origin',(0.04,-1.36,0.));
#4711=CARTESIAN_POINT('',(0.,-1.36,-0.08));
#4712=CARTESIAN_POINT('',(0.,-1.36,0.08));
#4713=CARTESIAN_POINT('Origin',(0.,-1.36,0.));
#4714=CARTESIAN_POINT('',(0.,-1.36,-0.04));
#4715=CARTESIAN_POINT('Origin',(0.,0.,-0.08));
#4716=CARTESIAN_POINT('',(0.,-1.6,0.08));
#4717=CARTESIAN_POINT('',(0.,0.,0.08));
#4718=CARTESIAN_POINT('',(0.,-1.6,-0.08));
#4719=CARTESIAN_POINT('',(0.,-1.6,-0.09));
#4720=CARTESIAN_POINT('',(0.,0.,-0.08));
#4721=CARTESIAN_POINT('Origin',(0.,0.,0.));
#4722=CARTESIAN_POINT('',(-0.08,-1.6,-9.79717439317883E-18));
#4723=CARTESIAN_POINT('Origin',(0.,-1.6,0.));
#4724=CARTESIAN_POINT('',(-0.08,0.,-9.79717439317883E-18));
#4725=CARTESIAN_POINT('Origin',(0.,-1.6,0.));
#4726=CARTESIAN_POINT('Origin',(-0.04,-1.6,0.));
#4727=CARTESIAN_POINT('',(0.,0.,0.));
#4728=CARTESIAN_POINT('',(0.,0.,0.));
#4729=CARTESIAN_POINT('',(0.,1.06,2.5));
#4730=CARTESIAN_POINT('',(0.,-1.06,2.5));
#4731=CARTESIAN_POINT('',(0.,0.9,2.5));
#4732=CARTESIAN_POINT('',(-0.4,-1.64,2.5));
#4733=CARTESIAN_POINT('',(0.,0.,0.));
#4734=CARTESIAN_POINT('',(0.435778713738291,6.2,-2.54902650954127));
#4735=CARTESIAN_POINT('',(0.435778713738291,0.3,7.48097349045873));
#4736=CARTESIAN_POINT('',(2.49048674522936,1.06,2.28211064313085));
#4737=CARTESIAN_POINT('',(2.49048674522936,-1.06,2.28211064313085));
#4738=CARTESIAN_POINT('',(2.49048674522936,0.9,2.28211064313085));
#4739=CARTESIAN_POINT('',(2.49048674522936,0.,-0.217889356869145));
#4740=CARTESIAN_POINT('',(2.09048674522936,-1.64,2.28211064313085));
#4741=CARTESIAN_POINT('',(0.,0.,0.));
#4742=CARTESIAN_POINT('',(15.5,0.,2.5));
#4743=CARTESIAN_POINT('',(13.,0.,2.5));
#4744=CARTESIAN_POINT('',(13.03,0.,2.5));
#4745=CARTESIAN_POINT('',(5.98369790806552,1.06,2.5));
#4746=CARTESIAN_POINT('',(5.98369790806552,-1.06,2.5));
#4747=CARTESIAN_POINT('',(5.98369790806552,0.9,2.5));
#4748=CARTESIAN_POINT('',(5.98369790806552,0.,0.));
#4749=CARTESIAN_POINT('',(5.58369790806552,-1.64,2.5));
#4750=CARTESIAN_POINT('',(0.,0.,0.));
#4751=CARTESIAN_POINT('',(0.,0.,0.));
#4752=CARTESIAN_POINT('',(0.,0.,0.));
#4753=CARTESIAN_POINT('',(0.,0.,0.));
#4754=UNCERTAINTY_MEASURE_WITH_UNIT(LENGTH_MEASURE(0.001),#4792,
'DISTANCE_ACCURACY_VALUE',
'Maximum model space distance between geometric entities at asserted c
onnectivities');
#4755=UNCERTAINTY_MEASURE_WITH_UNIT(LENGTH_MEASURE(0.001),#4792,
'DISTANCE_ACCURACY_VALUE',
'Maximum model space distance between geometric entities at asserted c
onnectivities');
#4756=UNCERTAINTY_MEASURE_WITH_UNIT(LENGTH_MEASURE(0.001),#4792,
'DISTANCE_ACCURACY_VALUE',
'Maximum model space distance between geometric entities at asserted c
onnectivities');
#4757=UNCERTAINTY_MEASURE_WITH_UNIT(LENGTH_MEASURE(0.001),#4792,
'DISTANCE_ACCURACY_VALUE',
'Maximum model space distance between geometric entities at asserted c
onnectivities');
#4758=UNCERTAINTY_MEASURE_WITH_UNIT(LENGTH_MEASURE(0.001),#4792,
'DISTANCE_ACCURACY_VALUE',
'Maximum model space distance between geometric entities at asserted c
onnectivities');
#4759=UNCERTAINTY_MEASURE_WITH_UNIT(LENGTH_MEASURE(0.001),#4792,
'DISTANCE_ACCURACY_VALUE',
'Maximum model space distance between geometric entities at asserted c
onnectivities');
#4760=UNCERTAINTY_MEASURE_WITH_UNIT(LENGTH_MEASURE(0.001),#4792,
'DISTANCE_ACCURACY_VALUE',
'Maximum model space distance between geometric entities at asserted c
onnectivities');
#4761=UNCERTAINTY_MEASURE_WITH_UNIT(LENGTH_MEASURE(0.001),#4792,
'DISTANCE_ACCURACY_VALUE',
'Maximum model space distance between geometric entities at asserted c
onnectivities');
#4762=UNCERTAINTY_MEASURE_WITH_UNIT(LENGTH_MEASURE(0.001),#4792,
'DISTANCE_ACCURACY_VALUE',
'Maximum model space distance between geometric entities at asserted c
onnectivities');
#4763=UNCERTAINTY_MEASURE_WITH_UNIT(LENGTH_MEASURE(0.001),#4792,
'DISTANCE_ACCURACY_VALUE',
'Maximum model space distance between geometric entities at asserted c
onnectivities');
#4764=UNCERTAINTY_MEASURE_WITH_UNIT(LENGTH_MEASURE(0.001),#4792,
'DISTANCE_ACCURACY_VALUE',
'Maximum model space distance between geometric entities at asserted c
onnectivities');
#4765=UNCERTAINTY_MEASURE_WITH_UNIT(LENGTH_MEASURE(0.001),#4792,
'DISTANCE_ACCURACY_VALUE',
'Maximum model space distance between geometric entities at asserted c
onnectivities');
#4766=UNCERTAINTY_MEASURE_WITH_UNIT(LENGTH_MEASURE(0.001),#4792,
'DISTANCE_ACCURACY_VALUE',
'Maximum model space distance between geometric entities at asserted c
onnectivities');
#4767=UNCERTAINTY_MEASURE_WITH_UNIT(LENGTH_MEASURE(0.001),#4792,
'DISTANCE_ACCURACY_VALUE',
'Maximum model space distance between geometric entities at asserted c
onnectivities');
#4768=UNCERTAINTY_MEASURE_WITH_UNIT(LENGTH_MEASURE(0.001),#4792,
'DISTANCE_ACCURACY_VALUE',
'Maximum model space distance between geometric entities at asserted c
onnectivities');
#4769=UNCERTAINTY_MEASURE_WITH_UNIT(LENGTH_MEASURE(0.001),#4792,
'DISTANCE_ACCURACY_VALUE',
'Maximum model space distance between geometric entities at asserted c
onnectivities');
#4770=UNCERTAINTY_MEASURE_WITH_UNIT(LENGTH_MEASURE(0.001),#4792,
'DISTANCE_ACCURACY_VALUE',
'Maximum model space distance between geometric entities at asserted c
onnectivities');
#4771=UNCERTAINTY_MEASURE_WITH_UNIT(LENGTH_MEASURE(0.001),#4792,
'DISTANCE_ACCURACY_VALUE',
'Maximum model space distance between geometric entities at asserted c
onnectivities');
#4772=UNCERTAINTY_MEASURE_WITH_UNIT(LENGTH_MEASURE(0.001),#4792,
'DISTANCE_ACCURACY_VALUE',
'Maximum model space distance between geometric entities at asserted c
onnectivities');
#4773=(
GEOMETRIC_REPRESENTATION_CONTEXT(3)
GLOBAL_UNCERTAINTY_ASSIGNED_CONTEXT((#4754))
GLOBAL_UNIT_ASSIGNED_CONTEXT((#4792,#4794,#4795))
REPRESENTATION_CONTEXT('','3D')
);
#4774=(
GEOMETRIC_REPRESENTATION_CONTEXT(3)
GLOBAL_UNCERTAINTY_ASSIGNED_CONTEXT((#4755))
GLOBAL_UNIT_ASSIGNED_CONTEXT((#4792,#4794,#4795))
REPRESENTATION_CONTEXT('','3D')
);
#4775=(
GEOMETRIC_REPRESENTATION_CONTEXT(3)
GLOBAL_UNCERTAINTY_ASSIGNED_CONTEXT((#4756))
GLOBAL_UNIT_ASSIGNED_CONTEXT((#4792,#4794,#4795))
REPRESENTATION_CONTEXT('','3D')
);
#4776=(
GEOMETRIC_REPRESENTATION_CONTEXT(3)
GLOBAL_UNCERTAINTY_ASSIGNED_CONTEXT((#4757))
GLOBAL_UNIT_ASSIGNED_CONTEXT((#4792,#4794,#4795))
REPRESENTATION_CONTEXT('','3D')
);
#4777=(
GEOMETRIC_REPRESENTATION_CONTEXT(3)
GLOBAL_UNCERTAINTY_ASSIGNED_CONTEXT((#4758))
GLOBAL_UNIT_ASSIGNED_CONTEXT((#4792,#4794,#4795))
REPRESENTATION_CONTEXT('','3D')
);
#4778=(
GEOMETRIC_REPRESENTATION_CONTEXT(3)
GLOBAL_UNCERTAINTY_ASSIGNED_CONTEXT((#4759))
GLOBAL_UNIT_ASSIGNED_CONTEXT((#4792,#4794,#4795))
REPRESENTATION_CONTEXT('','3D')
);
#4779=(
GEOMETRIC_REPRESENTATION_CONTEXT(3)
GLOBAL_UNCERTAINTY_ASSIGNED_CONTEXT((#4760))
GLOBAL_UNIT_ASSIGNED_CONTEXT((#4792,#4794,#4795))
REPRESENTATION_CONTEXT('','3D')
);
#4780=(
GEOMETRIC_REPRESENTATION_CONTEXT(3)
GLOBAL_UNCERTAINTY_ASSIGNED_CONTEXT((#4761))
GLOBAL_UNIT_ASSIGNED_CONTEXT((#4792,#4794,#4795))
REPRESENTATION_CONTEXT('','3D')
);
#4781=(
GEOMETRIC_REPRESENTATION_CONTEXT(3)
GLOBAL_UNCERTAINTY_ASSIGNED_CONTEXT((#4762))
GLOBAL_UNIT_ASSIGNED_CONTEXT((#4792,#4794,#4795))
REPRESENTATION_CONTEXT('','3D')
);
#4782=(
GEOMETRIC_REPRESENTATION_CONTEXT(3)
GLOBAL_UNCERTAINTY_ASSIGNED_CONTEXT((#4763))
GLOBAL_UNIT_ASSIGNED_CONTEXT((#4792,#4794,#4795))
REPRESENTATION_CONTEXT('','3D')
);
#4783=(
GEOMETRIC_REPRESENTATION_CONTEXT(3)
GLOBAL_UNCERTAINTY_ASSIGNED_CONTEXT((#4764))
GLOBAL_UNIT_ASSIGNED_CONTEXT((#4792,#4794,#4795))
REPRESENTATION_CONTEXT('','3D')
);
#4784=(
GEOMETRIC_REPRESENTATION_CONTEXT(3)
GLOBAL_UNCERTAINTY_ASSIGNED_CONTEXT((#4765))
GLOBAL_UNIT_ASSIGNED_CONTEXT((#4792,#4794,#4795))
REPRESENTATION_CONTEXT('','3D')
);
#4785=(
GEOMETRIC_REPRESENTATION_CONTEXT(3)
GLOBAL_UNCERTAINTY_ASSIGNED_CONTEXT((#4766))
GLOBAL_UNIT_ASSIGNED_CONTEXT((#4792,#4794,#4795))
REPRESENTATION_CONTEXT('','3D')
);
#4786=(
GEOMETRIC_REPRESENTATION_CONTEXT(3)
GLOBAL_UNCERTAINTY_ASSIGNED_CONTEXT((#4767))
GLOBAL_UNIT_ASSIGNED_CONTEXT((#4792,#4794,#4795))
REPRESENTATION_CONTEXT('','3D')
);
#4787=(
GEOMETRIC_REPRESENTATION_CONTEXT(3)
GLOBAL_UNCERTAINTY_ASSIGNED_CONTEXT((#4768))
GLOBAL_UNIT_ASSIGNED_CONTEXT((#4792,#4794,#4795))
REPRESENTATION_CONTEXT('','3D')
);
#4788=(
GEOMETRIC_REPRESENTATION_CONTEXT(3)
GLOBAL_UNCERTAINTY_ASSIGNED_CONTEXT((#4769))
GLOBAL_UNIT_ASSIGNED_CONTEXT((#4792,#4794,#4795))
REPRESENTATION_CONTEXT('','3D')
);
#4789=(
GEOMETRIC_REPRESENTATION_CONTEXT(3)
GLOBAL_UNCERTAINTY_ASSIGNED_CONTEXT((#4770))
GLOBAL_UNIT_ASSIGNED_CONTEXT((#4792,#4794,#4795))
REPRESENTATION_CONTEXT('','3D')
);
#4790=(
GEOMETRIC_REPRESENTATION_CONTEXT(3)
GLOBAL_UNCERTAINTY_ASSIGNED_CONTEXT((#4771))
GLOBAL_UNIT_ASSIGNED_CONTEXT((#4792,#4794,#4795))
REPRESENTATION_CONTEXT('','3D')
);
#4791=(
GEOMETRIC_REPRESENTATION_CONTEXT(3)
GLOBAL_UNCERTAINTY_ASSIGNED_CONTEXT((#4772))
GLOBAL_UNIT_ASSIGNED_CONTEXT((#4792,#4794,#4795))
REPRESENTATION_CONTEXT('','3D')
);
#4792=(
LENGTH_UNIT()
NAMED_UNIT(*)
SI_UNIT(.CENTI.,.METRE.)
);
#4793=(
LENGTH_UNIT()
NAMED_UNIT(*)
SI_UNIT($,.METRE.)
);
#4794=(
NAMED_UNIT(*)
PLANE_ANGLE_UNIT()
SI_UNIT($,.RADIAN.)
);
#4795=(
NAMED_UNIT(*)
SI_UNIT($,.STERADIAN.)
SOLID_ANGLE_UNIT()
);
#4796=SHAPE_DEFINITION_REPRESENTATION(#4814,#4860);
#4797=SHAPE_DEFINITION_REPRESENTATION(#4815,#4861);
#4798=SHAPE_DEFINITION_REPRESENTATION(#4816,#4862);
#4799=SHAPE_DEFINITION_REPRESENTATION(#4817,#4863);
#4800=SHAPE_DEFINITION_REPRESENTATION(#4818,#4864);
#4801=SHAPE_DEFINITION_REPRESENTATION(#4819,#4865);
#4802=SHAPE_DEFINITION_REPRESENTATION(#4820,#4866);
#4803=SHAPE_DEFINITION_REPRESENTATION(#4821,#4867);
#4804=SHAPE_DEFINITION_REPRESENTATION(#4822,#4868);
#4805=SHAPE_DEFINITION_REPRESENTATION(#4824,#4869);
#4806=SHAPE_DEFINITION_REPRESENTATION(#4825,#4870);
#4807=SHAPE_DEFINITION_REPRESENTATION(#4826,#4871);
#4808=SHAPE_DEFINITION_REPRESENTATION(#4827,#4872);
#4809=SHAPE_DEFINITION_REPRESENTATION(#4828,#4873);
#4810=SHAPE_DEFINITION_REPRESENTATION(#4829,#4874);
#4811=SHAPE_DEFINITION_REPRESENTATION(#4830,#4875);
#4812=SHAPE_DEFINITION_REPRESENTATION(#4831,#4876);
#4813=SHAPE_DEFINITION_REPRESENTATION(#4832,#4877);
#4814=PRODUCT_DEFINITION_SHAPE('',$,#4879);
#4815=PRODUCT_DEFINITION_SHAPE('',$,#4880);
#4816=PRODUCT_DEFINITION_SHAPE('',$,#4881);
#4817=PRODUCT_DEFINITION_SHAPE('',$,#4882);
#4818=PRODUCT_DEFINITION_SHAPE('',$,#4883);
#4819=PRODUCT_DEFINITION_SHAPE('',$,#4884);
#4820=PRODUCT_DEFINITION_SHAPE('',$,#4885);
#4821=PRODUCT_DEFINITION_SHAPE('',$,#4886);
#4822=PRODUCT_DEFINITION_SHAPE('',$,#4887);
#4823=PRODUCT_DEFINITION_SHAPE($,$,#120);
#4824=PRODUCT_DEFINITION_SHAPE('',$,#4888);
#4825=PRODUCT_DEFINITION_SHAPE('',$,#4889);
#4826=PRODUCT_DEFINITION_SHAPE('',$,#4890);
#4827=PRODUCT_DEFINITION_SHAPE('',$,#4891);
#4828=PRODUCT_DEFINITION_SHAPE('',$,#4892);
#4829=PRODUCT_DEFINITION_SHAPE('',$,#4893);
#4830=PRODUCT_DEFINITION_SHAPE('',$,#4894);
#4831=PRODUCT_DEFINITION_SHAPE('',$,#4895);
#4832=PRODUCT_DEFINITION_SHAPE('',$,#4896);
#4833=PRODUCT_DEFINITION_SHAPE($,$,#121);
#4834=PRODUCT_DEFINITION_SHAPE($,$,#122);
#4835=PRODUCT_DEFINITION_SHAPE($,$,#123);
#4836=PRODUCT_DEFINITION_SHAPE($,$,#124);
#4837=PRODUCT_DEFINITION_SHAPE($,$,#125);
#4838=PRODUCT_DEFINITION_SHAPE($,$,#126);
#4839=PRODUCT_DEFINITION_SHAPE($,$,#127);
#4840=PRODUCT_DEFINITION_SHAPE($,$,#128);
#4841=PRODUCT_DEFINITION_SHAPE($,$,#129);
#4842=PRODUCT_DEFINITION_SHAPE($,$,#130);
#4843=PRODUCT_DEFINITION_SHAPE($,$,#131);
#4844=PRODUCT_DEFINITION_SHAPE($,$,#132);
#4845=PRODUCT_DEFINITION_SHAPE($,$,#133);
#4846=PRODUCT_DEFINITION_SHAPE($,$,#134);
#4847=PRODUCT_DEFINITION_SHAPE($,$,#135);
#4848=PRODUCT_DEFINITION_SHAPE($,$,#136);
#4849=PRODUCT_DEFINITION_SHAPE($,$,#137);
#4850=PRODUCT_DEFINITION_SHAPE($,$,#138);
#4851=PRODUCT_DEFINITION_SHAPE($,$,#139);
#4852=PRODUCT_DEFINITION_SHAPE($,$,#140);
#4853=PRODUCT_DEFINITION_SHAPE($,$,#141);
#4854=PRODUCT_DEFINITION_SHAPE($,$,#142);
#4855=PRODUCT_DEFINITION_SHAPE($,$,#143);
#4856=PRODUCT_DEFINITION_SHAPE($,$,#144);
#4857=PRODUCT_DEFINITION_SHAPE($,$,#145);
#4858=PRODUCT_DEFINITION_SHAPE($,$,#146);
#4859=PRODUCT_DEFINITION_SHAPE($,$,#147);
#4860=SHAPE_REPRESENTATION('',(#2787,#3066,#3067,#3068,#3069),#4773);
#4861=SHAPE_REPRESENTATION('',(#2788,#3043,#3044,#3045,#3046,#3047,#3048),
#4774);
#4862=SHAPE_REPRESENTATION('',(#2789),#4775);
#4863=SHAPE_REPRESENTATION('',(#2837,#3049,#3050,#3051,#3052,#3053,#3054,
#3055,#3056),#4776);
#4864=SHAPE_REPRESENTATION('',(#2838),#4777);
#4865=SHAPE_REPRESENTATION('',(#2881),#4778);
#4866=SHAPE_REPRESENTATION('',(#2891),#4779);
#4867=SHAPE_REPRESENTATION('',(#2915,#2933),#4780);
#4868=SHAPE_REPRESENTATION('',(#2916),#4781);
#4869=SHAPE_REPRESENTATION('',(#2934,#3057,#3058,#3059,#3060,#3061,#3062,
#3063,#3064,#3065),#4782);
#4870=SHAPE_REPRESENTATION('',(#2935),#4783);
#4871=SHAPE_REPRESENTATION('',(#2960),#4784);
#4872=SHAPE_REPRESENTATION('',(#2977),#4785);
#4873=SHAPE_REPRESENTATION('',(#2993),#4786);
#4874=SHAPE_REPRESENTATION('',(#2999),#4787);
#4875=SHAPE_REPRESENTATION('',(#3014),#4788);
#4876=SHAPE_REPRESENTATION('',(#3023),#4789);
#4877=SHAPE_REPRESENTATION('',(#3032),#4790);
#4878=PRODUCT_DEFINITION_CONTEXT('part definition',#4934,'design');
#4879=PRODUCT_DEFINITION('PAT-058',
'PAT-058',#4897,#4878);
#4880=PRODUCT_DEFINITION('Base guide and handle stop',
'Base guide and handle stop',#4898,#4878);
#4881=PRODUCT_DEFINITION('Twenty-five millimetre clamp base',
'Twenty-five millimetre clamp base',#4899,#4878);
#4882=PRODUCT_DEFINITION('Operating crank','Operating crank',#4900,#4878);
#4883=PRODUCT_DEFINITION('Operating lever','Operating lever',#4901,#4878);
#4884=PRODUCT_DEFINITION('Handle','Handle',#4902,#4878);
#4885=PRODUCT_DEFINITION('M5x14 Cap Screw','M5x14 Cap Screw',#4903,#4878);
#4886=PRODUCT_DEFINITION('Toggle connecting link',
'Toggle connecting link',#4904,#4878);
#4887=PRODUCT_DEFINITION('Thirty-five millimetre toggle link',
'Thirty-five millimetre toggle link',#4905,#4878);
#4888=PRODUCT_DEFINITION('Plunger and M8 spindle',
'Plunger and M8 spindle',#4906,#4878);
#4889=PRODUCT_DEFINITION('Forked pressure plunger',
'Forked pressure plunger',#4907,#4878);
#4890=PRODUCT_DEFINITION('Hex Bolt - M8x40','Hex Bolt - M8x40',#4908,#4878);
#4891=PRODUCT_DEFINITION('Hex Nut - M8','Hex Nut - M8',#4909,#4878);
#4892=PRODUCT_DEFINITION('Elastomer pressure pad installed',
'Elastomer pressure pad installed',#4910,#4878);
#4893=PRODUCT_DEFINITION('Clevis Pin - 6x30','Clevis Pin - 6x30',#4911,
#4878);
#4894=PRODUCT_DEFINITION('Flat Washer - M6','Flat Washer - M6',#4912,#4878);
#4895=PRODUCT_DEFINITION('Pivot retention spacer',
'Pivot retention spacer',#4913,#4878);
#4896=PRODUCT_DEFINITION('Split Pin - 1.6x16','Split Pin - 1.6x16',#4914,
#4878);
#4897=PRODUCT_DEFINITION_FORMATION('',$,#4936);
#4898=PRODUCT_DEFINITION_FORMATION('',$,#4937);
#4899=PRODUCT_DEFINITION_FORMATION('',$,#4938);
#4900=PRODUCT_DEFINITION_FORMATION('',$,#4939);
#4901=PRODUCT_DEFINITION_FORMATION('',$,#4940);
#4902=PRODUCT_DEFINITION_FORMATION('',$,#4941);
#4903=PRODUCT_DEFINITION_FORMATION('',$,#4942);
#4904=PRODUCT_DEFINITION_FORMATION('',$,#4943);
#4905=PRODUCT_DEFINITION_FORMATION('',$,#4944);
#4906=PRODUCT_DEFINITION_FORMATION('',$,#4945);
#4907=PRODUCT_DEFINITION_FORMATION('',$,#4946);
#4908=PRODUCT_DEFINITION_FORMATION('',$,#4947);
#4909=PRODUCT_DEFINITION_FORMATION('',$,#4948);
#4910=PRODUCT_DEFINITION_FORMATION('',$,#4949);
#4911=PRODUCT_DEFINITION_FORMATION('',$,#4950);
#4912=PRODUCT_DEFINITION_FORMATION('',$,#4951);
#4913=PRODUCT_DEFINITION_FORMATION('',$,#4952);
#4914=PRODUCT_DEFINITION_FORMATION('',$,#4953);
#4915=PRODUCT_RELATED_PRODUCT_CATEGORY('PAT-058','PAT-058',(#4936));
#4916=PRODUCT_RELATED_PRODUCT_CATEGORY('Base guide and handle stop',
'Base guide and handle stop',(#4937));
#4917=PRODUCT_RELATED_PRODUCT_CATEGORY(
'Twenty-five millimetre clamp base','Twenty-five millimetre clamp base',
(#4938));
#4918=PRODUCT_RELATED_PRODUCT_CATEGORY('Operating crank',
'Operating crank',(#4939));
#4919=PRODUCT_RELATED_PRODUCT_CATEGORY('Operating lever',
'Operating lever',(#4940));
#4920=PRODUCT_RELATED_PRODUCT_CATEGORY('Handle','Handle',(#4941));
#4921=PRODUCT_RELATED_PRODUCT_CATEGORY('M5x14 Cap Screw',
'M5x14 Cap Screw',(#4942));
#4922=PRODUCT_RELATED_PRODUCT_CATEGORY('Toggle connecting link',
'Toggle connecting link',(#4943));
#4923=PRODUCT_RELATED_PRODUCT_CATEGORY(
'Thirty-five millimetre toggle link',
'Thirty-five millimetre toggle link',(#4944));
#4924=PRODUCT_RELATED_PRODUCT_CATEGORY('Plunger and M8 spindle',
'Plunger and M8 spindle',(#4945));
#4925=PRODUCT_RELATED_PRODUCT_CATEGORY('Forked pressure plunger',
'Forked pressure plunger',(#4946));
#4926=PRODUCT_RELATED_PRODUCT_CATEGORY('Hex Bolt - M8x40',
'Hex Bolt - M8x40',(#4947));
#4927=PRODUCT_RELATED_PRODUCT_CATEGORY('Hex Nut - M8','Hex Nut - M8',(#4948));
#4928=PRODUCT_RELATED_PRODUCT_CATEGORY(
'Elastomer pressure pad installed','Elastomer pressure pad installed',(#4949));
#4929=PRODUCT_RELATED_PRODUCT_CATEGORY('Clevis Pin - 6x30',
'Clevis Pin - 6x30',(#4950));
#4930=PRODUCT_RELATED_PRODUCT_CATEGORY('Flat Washer - M6',
'Flat Washer - M6',(#4951));
#4931=PRODUCT_RELATED_PRODUCT_CATEGORY('Pivot retention spacer',
'Pivot retention spacer',(#4952));
#4932=PRODUCT_RELATED_PRODUCT_CATEGORY('Split Pin - 1.6x16',
'Split Pin - 1.6x16',(#4953));
#4933=APPLICATION_PROTOCOL_DEFINITION('international standard',
'automotive_design',2009,#4934);
#4934=APPLICATION_CONTEXT(
'Core Data for Automotive Mechanical Design Process');
#4935=PRODUCT_CONTEXT('part definition',#4934,'mechanical');
#4936=PRODUCT('PAT-058','PAT-058',
'PAT-058',(#4935));
#4937=PRODUCT('Base guide and handle stop','Base guide and handle stop',
'Base guide and handle stop',(#4935));
#4938=PRODUCT('Twenty-five millimetre clamp base',
'Twenty-five millimetre clamp base','Twenty-five millimetre clamp base',
(#4935));
#4939=PRODUCT('Operating crank','Operating crank','Operating crank',(#4935));
#4940=PRODUCT('Operating lever','Operating lever','Operating lever',(#4935));
#4941=PRODUCT('Handle','Handle','Handle',(#4935));
#4942=PRODUCT('M5x14 Cap Screw','M5x14 Cap Screw','M5x14 Cap Screw',(#4935));
#4943=PRODUCT('Toggle connecting link','Toggle connecting link',
'Toggle connecting link',(#4935));
#4944=PRODUCT('Thirty-five millimetre toggle link',
'Thirty-five millimetre toggle link',
'Thirty-five millimetre toggle link',(#4935));
#4945=PRODUCT('Plunger and M8 spindle','Plunger and M8 spindle',
'Plunger and M8 spindle',(#4935));
#4946=PRODUCT('Forked pressure plunger','Forked pressure plunger',
'Forked pressure plunger',(#4935));
#4947=PRODUCT('Hex Bolt - M8x40','Hex Bolt - M8x40','Hex Bolt - M8x40',
(#4935));
#4948=PRODUCT('Hex Nut - M8','Hex Nut - M8','Hex Nut - M8',(#4935));
#4949=PRODUCT('Elastomer pressure pad installed',
'Elastomer pressure pad installed','Elastomer pressure pad installed',(#4935));
#4950=PRODUCT('Clevis Pin - 6x30','Clevis Pin - 6x30',
'Clevis Pin - 6x30',(#4935));
#4951=PRODUCT('Flat Washer - M6','Flat Washer - M6','Flat Washer - M6',
(#4935));
#4952=PRODUCT('Pivot retention spacer','Pivot retention spacer',
'Pivot retention spacer',(#4935));
#4953=PRODUCT('Split Pin - 1.6x16','Split Pin - 1.6x16',
'Split Pin - 1.6x16',(#4935));
#4954=PRESENTATION_STYLE_ASSIGNMENT((#4960));
#4955=PRESENTATION_STYLE_ASSIGNMENT((#4961));
#4956=PRESENTATION_STYLE_ASSIGNMENT((#4962));
#4957=PRESENTATION_STYLE_ASSIGNMENT((#4963));
#4958=PRESENTATION_STYLE_ASSIGNMENT((#4964));
#4959=PRESENTATION_STYLE_ASSIGNMENT((#4965));
#4960=SURFACE_STYLE_USAGE(.BOTH.,#4966);
#4961=SURFACE_STYLE_USAGE(.BOTH.,#4967);
#4962=SURFACE_STYLE_USAGE(.BOTH.,#4968);
#4963=SURFACE_STYLE_USAGE(.BOTH.,#4969);
#4964=SURFACE_STYLE_USAGE(.BOTH.,#4970);
#4965=SURFACE_STYLE_USAGE(.BOTH.,#4971);
#4966=SURFACE_SIDE_STYLE('',(#4972));
#4967=SURFACE_SIDE_STYLE('',(#4973));
#4968=SURFACE_SIDE_STYLE('',(#4974));
#4969=SURFACE_SIDE_STYLE('',(#4975));
#4970=SURFACE_SIDE_STYLE('',(#4976));
#4971=SURFACE_SIDE_STYLE('',(#4977));
#4972=SURFACE_STYLE_FILL_AREA(#4978);
#4973=SURFACE_STYLE_FILL_AREA(#4979);
#4974=SURFACE_STYLE_FILL_AREA(#4980);
#4975=SURFACE_STYLE_FILL_AREA(#4981);
#4976=SURFACE_STYLE_FILL_AREA(#4982);
#4977=SURFACE_STYLE_FILL_AREA(#4983);
#4978=FILL_AREA_STYLE('Steel - Satin',(#4984));
#4979=FILL_AREA_STYLE('CAD Library Painted - Deep blue',(#4985));
#4980=FILL_AREA_STYLE('CAD Library Painted - Light blue',(#4986));
#4981=FILL_AREA_STYLE('CAD Library Painted - Graphite',(#4987));
#4982=FILL_AREA_STYLE('CAD Library Painted - Engineering blue',(#4988));
#4983=FILL_AREA_STYLE('CAD Library Painted - Steel gray',(#4989));
#4984=FILL_AREA_STYLE_COLOUR('Steel - Satin',#4990);
#4985=FILL_AREA_STYLE_COLOUR('CAD Library Painted - Deep blue',#4991);
#4986=FILL_AREA_STYLE_COLOUR('CAD Library Painted - Light blue',#4992);
#4987=FILL_AREA_STYLE_COLOUR('CAD Library Painted - Graphite',#4993);
#4988=FILL_AREA_STYLE_COLOUR('CAD Library Painted - Engineering blue',#4994);
#4989=FILL_AREA_STYLE_COLOUR('CAD Library Painted - Steel gray',#4995);
#4990=COLOUR_RGB('Steel - Satin',0.627450980392157,0.627450980392157,0.627450980392157);
#4991=COLOUR_RGB('CAD Library Painted - Deep blue',0.0784313725490196,0.203921568627451,
0.349019607843137);
#4992=COLOUR_RGB('CAD Library Painted - Light blue',0.286274509803922,0.552941176470588,
0.780392156862745);
#4993=COLOUR_RGB('CAD Library Painted - Graphite',0.0980392156862745,0.109803921568627,
0.125490196078431);
#4994=COLOUR_RGB('CAD Library Painted - Engineering blue',0.12156862745098,
0.356862745098039,0.6);
#4995=COLOUR_RGB('CAD Library Painted - Steel gray',0.592156862745098,0.631372549019608,
0.67843137254902);
#4996=COLOUR_RGB('Dark Blue',0.08,0.2,0.34);
#4997=FILL_AREA_STYLE_COLOUR('',#4996);
#4998=FILL_AREA_STYLE('',(#4997));
#4999=SURFACE_STYLE_FILL_AREA(#4998);
#5000=SURFACE_SIDE_STYLE('',(#4999));
#5001=SURFACE_STYLE_USAGE(.BOTH.,#5000);
#5002=PRESENTATION_STYLE_ASSIGNMENT((#5001));
#5003=COLOUR_RGB('Light Blue',0.38,0.62,0.78);
#5004=FILL_AREA_STYLE_COLOUR('',#5003);
#5005=FILL_AREA_STYLE('',(#5004));
#5006=SURFACE_STYLE_FILL_AREA(#5005);
#5007=SURFACE_SIDE_STYLE('',(#5006));
#5008=SURFACE_STYLE_USAGE(.BOTH.,#5007);
#5009=PRESENTATION_STYLE_ASSIGNMENT((#5008));
#5010=COLOUR_RGB('Sky Blue',0.24,0.69,0.87);
#5011=FILL_AREA_STYLE_COLOUR('',#5010);
#5012=FILL_AREA_STYLE('',(#5011));
#5013=SURFACE_STYLE_FILL_AREA(#5012);
#5014=SURFACE_SIDE_STYLE('',(#5013));
#5015=SURFACE_STYLE_USAGE(.BOTH.,#5014);
#5016=PRESENTATION_STYLE_ASSIGNMENT((#5015));
#5017=COLOUR_RGB('Grey',0.48,0.52,0.57);
#5018=FILL_AREA_STYLE_COLOUR('',#5017);
#5019=FILL_AREA_STYLE('',(#5018));
#5020=SURFACE_STYLE_FILL_AREA(#5019);
#5021=SURFACE_SIDE_STYLE('',(#5020));
#5022=SURFACE_STYLE_USAGE(.BOTH.,#5021);
#5023=PRESENTATION_STYLE_ASSIGNMENT((#5022));
#5024=COLOUR_RGB('Black',0.12,0.14,0.17);
#5025=FILL_AREA_STYLE_COLOUR('',#5024);
#5026=FILL_AREA_STYLE('',(#5025));
#5027=SURFACE_STYLE_FILL_AREA(#5026);
#5028=SURFACE_SIDE_STYLE('',(#5027));
#5029=SURFACE_STYLE_USAGE(.BOTH.,#5028);
#5030=PRESENTATION_STYLE_ASSIGNMENT((#5029));
#5031=COLOUR_RGB('Off White',0.89,0.88,0.83);
#5032=FILL_AREA_STYLE_COLOUR('',#5031);
#5033=FILL_AREA_STYLE('',(#5032));
#5034=SURFACE_STYLE_FILL_AREA(#5033);
#5035=SURFACE_SIDE_STYLE('',(#5034));
#5036=SURFACE_STYLE_USAGE(.BOTH.,#5035);
#5037=PRESENTATION_STYLE_ASSIGNMENT((#5036));
ENDSEC;
END-ISO-10303-21;
